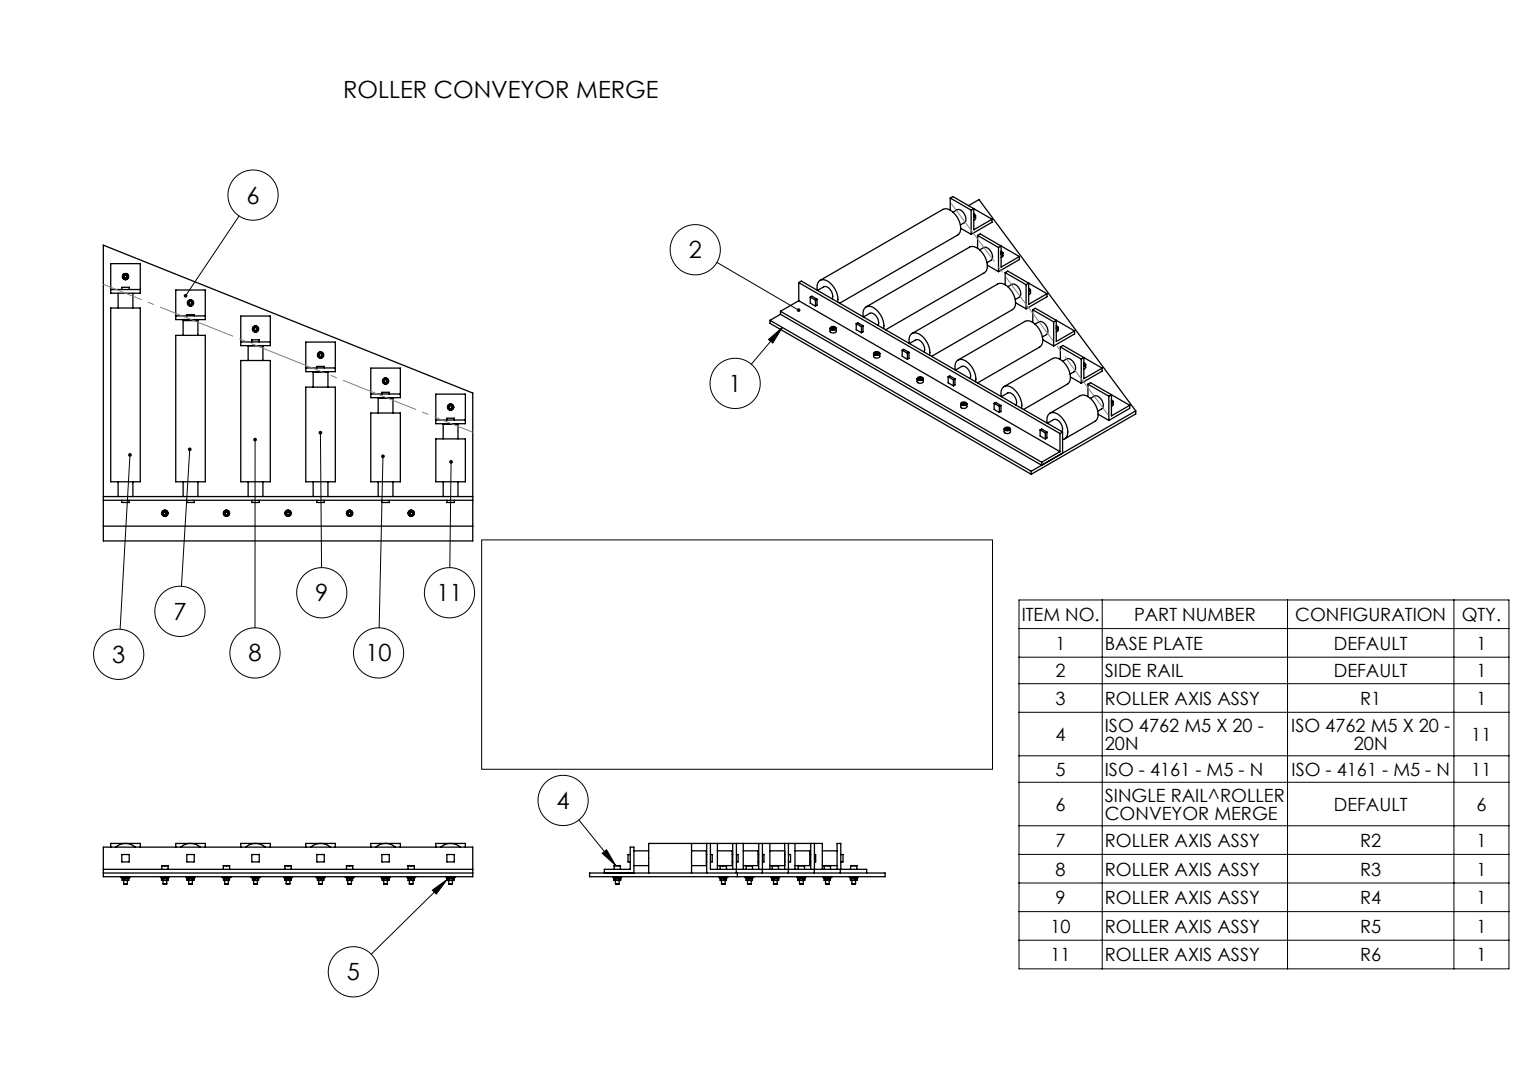
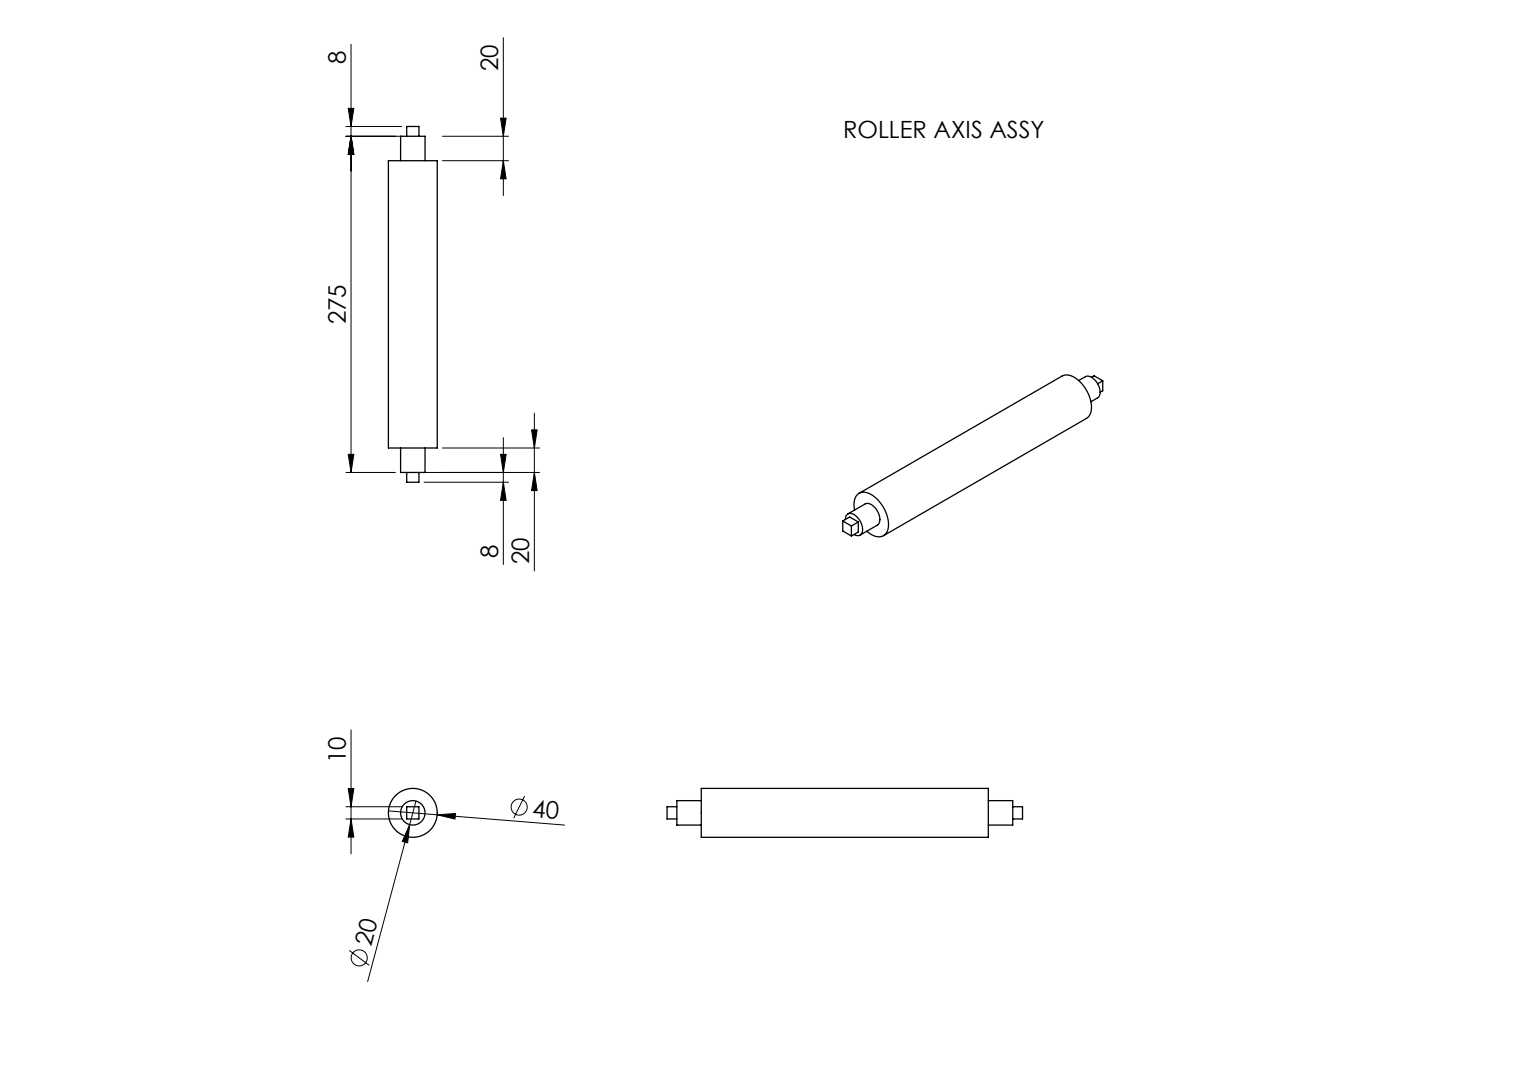
ISO-10303-21;
HEADER;
FILE_DESCRIPTION (('STEP AP214'),
    '1' );
FILE_NAME ('MAS-188',
    '2026-10-24T11:01:53',
    ( '' ),
    ( '' ),
    'SwSTEP 2.0',
    'SolidWorks 2026',
    '' );
FILE_SCHEMA (( 'AUTOMOTIVE_DESIGN' ));
ENDSEC;

DATA;
#1 = FACE_OUTER_BOUND ( 'NONE', #2167, .T. ) ;
#2 = DIRECTION ( 'NONE',  ( 0.000000000000000000, 0.000000000000000000, 1.000000000000000000 ) ) ;
#3 = CARTESIAN_POINT ( 'NONE',  ( 0.000000000000000000, 0.000000000000000000, -4.694516984716113228 ) ) ;
#4 = FILL_AREA_STYLE_COLOUR ( '', #2186 ) ;
#5 = ORIENTED_EDGE ( 'NONE', *, *, #5962, .F. ) ;
#6 = ORIENTED_EDGE ( 'NONE', *, *, #8549, .T. ) ;
#7 = EDGE_CURVE ( 'NONE', #1026, #1114, #8022, .T. ) ;
#8 = ORIENTED_EDGE ( 'NONE', *, *, #6474, .F. ) ;
#9 = APPLICATION_CONTEXT ( 'automotive_design' ) ;
#10 = LINE ( 'NONE', #1868, #5341 ) ;
#11 = EDGE_CURVE ( 'NONE', #6628, #4697, #895, .T. ) ;
#12 = CARTESIAN_POINT ( 'NONE',  ( -5.000000000000000000, -5.000000000000000000, 148.0000000000000284 ) ) ;
#13 = PRODUCT_DEFINITION_FORMATION_WITH_SPECIFIED_SOURCE ( 'ANY', '', #8583, .NOT_KNOWN. ) ;
#14 = EDGE_CURVE ( 'NONE', #3511, #8141, #5542, .T. ) ;
#15 = DIRECTION ( 'NONE',  ( 1.000000000000000000, 0.000000000000000000, 0.000000000000000000 ) ) ;
#16 = ORIENTED_EDGE ( 'NONE', *, *, #5135, .F. ) ;
#17 = LINE ( 'NONE', #599, #1287 ) ;
#18 = CARTESIAN_POINT ( 'NONE',  ( 386.6666666666666288, -15.00000000000000000, 165.1500000000000625 ) ) ;
#19 = FACE_BOUND ( 'NONE', #2899, .T. ) ;
#20 = CARTESIAN_POINT ( 'NONE',  ( 176.0000000000000000, -30.00000000000000355, -86.63142504031549151 ) ) ;
#21 = LINE ( 'NONE', #519, #5740 ) ;
#22 = ORIENTED_EDGE ( 'NONE', *, *, #3719, .T. ) ;
#23 = AXIS2_PLACEMENT_3D ( 'NONE', #2020, #5963, #7409 ) ;
#24 = VERTEX_POINT ( 'NONE', #6412 ) ;
#25 = DIRECTION ( 'NONE',  ( 0.000000000000000000, 0.000000000000000000, 1.000000000000000000 ) ) ;
#26 = CARTESIAN_POINT ( 'NONE',  ( -30.00000000000000000, 15.00000000000000000, 145.0000000000000284 ) ) ;
#27 = AXIS2_PLACEMENT_3D ( 'NONE', #2373, #401, #2287 ) ;
#28 = VECTOR ( 'NONE', #6395, 1000.000000000000000 ) ;
#29 = LINE ( 'NONE', #6648, #3973 ) ;
#30 = EDGE_CURVE ( 'NONE', #66, #5441, #6753, .T. ) ;
#31 = CARTESIAN_POINT ( 'NONE',  ( -4.999999999999998224, -4.999999999999998224, 145.0000000000000284 ) ) ;
#32 = ORIENTED_EDGE ( 'NONE', *, *, #8020, .T. ) ;
#33=STYLED_ITEM('',(#8671),#7573);
#34 = CIRCLE ( 'NONE', #8257, 2.649999999999985700 ) ;
#35 = VERTEX_POINT ( 'NONE', #5063 ) ;
#36 = LINE ( 'NONE', #1308, #2826 ) ;
#37 = AXIS2_PLACEMENT_3D ( 'NONE', #3813, #3117, #8346 ) ;
#38 = MECHANICAL_DESIGN_GEOMETRIC_PRESENTATION_REPRESENTATION (  '', ( #7560 ), #3810 ) ;
#39 = CARTESIAN_POINT ( 'NONE',  ( 264.0000000000000000, -20.00000000000000000, -48.78142504031547588 ) ) ;
#40 = DIRECTION ( 'NONE',  ( 1.000000000000000000, 0.000000000000000000, 0.000000000000000000 ) ) ;
#41 = ORIENTED_EDGE ( 'NONE', *, *, #7818, .F. ) ;
#42 = DIRECTION ( 'NONE',  ( -0.000000000000000000, -0.000000000000000000, 1.000000000000000000 ) ) ;
#43 = VECTOR ( 'NONE', #8305, 1000.000000000000000 ) ;
#44 = DIRECTION ( 'NONE',  ( -1.000000000000000000, 0.000000000000000000, 0.000000000000000000 ) ) ;
#45 = CARTESIAN_POINT ( 'NONE',  ( 352.0000000000000000, -25.00000000000000000, -18.88142504031545243 ) ) ;
#46 = AXIS2_PLACEMENT_3D ( 'NONE', #70, #7390, #6602 ) ;
#47 = CARTESIAN_POINT ( 'NONE',  ( 5.000000000000000000, -5.000000000000000000, 148.0000000000000284 ) ) ;
#48 = VECTOR ( 'NONE', #1988, 1000.000000000000000 ) ;
#49 = CARTESIAN_POINT ( 'NONE',  ( 20.00000000000000000, 0.000000000000000000, 120.0000000000000142 ) ) ;
#50 = DIRECTION ( 'NONE',  ( -0.000000000000000000, 1.000000000000000000, -0.000000000000000000 ) ) ;
#51 = EDGE_LOOP ( 'NONE', ( #1765, #1748 ) ) ;
#52 = EDGE_LOOP ( 'NONE', ( #3037, #7373 ) ) ;
#53 = UNCERTAINTY_MEASURE_WITH_UNIT (LENGTH_MEASURE( 1.000000000000000082E-05 ), #4971, 'distance_accuracy_value', 'NONE');
#54 = VERTEX_POINT ( 'NONE', #1769 ) ;
#55 = DIRECTION ( 'NONE',  ( 1.734723475976806848E-16, -1.000000000000000000, -0.000000000000000000 ) ) ;
#56 = CARTESIAN_POINT ( 'NONE',  ( 10.00000000000000000, 0.000000000000000000, 140.0000000000000000 ) ) ;
#57 = ADVANCED_FACE ( 'NONE', ( #4416 ), #7068, .T. ) ;
#58 = VERTEX_POINT ( 'NONE', #5981 ) ;
#59 = CARTESIAN_POINT ( 'NONE',  ( 5.000000000000000000, -5.000000000000000000, 7.000000000000006217 ) ) ;
#60 = EDGE_CURVE ( 'NONE', #24, #4191, #63, .T. ) ;
#61 = ORIENTED_EDGE ( 'NONE', *, *, #1740, .F. ) ;
#62 = LINE ( 'NONE', #7469, #2279 ) ;
#63 = LINE ( 'NONE', #5464, #2595 ) ;
#64 = CARTESIAN_POINT ( 'NONE',  ( 176.0000000000000000, -10.00000000000000178, -86.63142504031549151 ) ) ;
#65 =( NAMED_UNIT ( * ) PLANE_ANGLE_UNIT ( ) SI_UNIT ( $, .RADIAN. ) );
#66 = VERTEX_POINT ( 'NONE', #8006 ) ;
#67 = EDGE_CURVE ( 'NONE', #3923, #3144, #6728, .T. ) ;
#68 = ORIENTED_EDGE ( 'NONE', *, *, #4489, .T. ) ;
#69 = LINE ( 'NONE', #4867, #7268 ) ;
#70 = CARTESIAN_POINT ( 'NONE',  ( 219.9999999999999716, -14.99999999999999822, 162.5000000000000853 ) ) ;
#71 = CIRCLE ( 'NONE', #3416, 10.00000000000000000 ) ;
#72 = DIRECTION ( 'NONE',  ( 0.000000000000000000, 0.000000000000000000, 1.000000000000000000 ) ) ;
#73 = CARTESIAN_POINT ( 'NONE',  ( 0.000000000000000000, 0.000000000000000000, 140.0000000000000000 ) ) ;
#74 = EDGE_LOOP ( 'NONE', ( #3526, #1411, #5391, #5718 ) ) ;
#75 = CIRCLE ( 'NONE', #7173, 10.00000000000000000 ) ;
#76 = AXIS2_PLACEMENT_3D ( 'NONE', #4160, #6813, #4641 ) ;
#77 = LINE ( 'NONE', #5562, #6140 ) ;
#78 = ORIENTED_EDGE ( 'NONE', *, *, #2299, .F. ) ;
#79 = DIRECTION ( 'NONE',  ( 0.000000000000000000, 0.000000000000000000, 1.000000000000000000 ) ) ;
#80 = CIRCLE ( 'NONE', #1767, 2.649999999999985700 ) ;
#81 = VECTOR ( 'NONE', #7075, 1000.000000000000000 ) ;
#82 = FACE_OUTER_BOUND ( 'NONE', #3870, .T. ) ;
#83 = DIRECTION ( 'NONE',  ( 0.000000000000000000, 1.000000000000000000, -1.224646799147353207E-16 ) ) ;
#84 = ORIENTED_EDGE ( 'NONE', *, *, #5741, .T. ) ;
#85 = DIRECTION ( 'NONE',  ( 0.000000000000000000, 1.000000000000000000, 0.000000000000000000 ) ) ;
#86 = DIRECTION ( 'NONE',  ( -0.000000000000000000, -0.000000000000000000, -1.000000000000000000 ) ) ;
#87 = ADVANCED_FACE ( 'NONE', ( #7344 ), #1423, .F. ) ;
#88 = EDGE_CURVE ( 'NONE', #3290, #1917, #5360, .T. ) ;
#89 = DIRECTION ( 'NONE',  ( -1.000000000000000000, 0.000000000000000000, -0.000000000000000000 ) ) ;
#90 = ADVANCED_FACE ( 'NONE', ( #2733 ), #143, .T. ) ;
#91 = CARTESIAN_POINT ( 'NONE',  ( 0.000000000000000000, 0.000000000000000000, -0.2800830152838844622 ) ) ;
#92 = DIRECTION ( 'NONE',  ( 1.000000000000000000, 0.000000000000000000, 0.000000000000000000 ) ) ;
#93 = FACE_OUTER_BOUND ( 'NONE', #2661, .T. ) ;
#94 = ORIENTED_EDGE ( 'NONE', *, *, #7928, .T. ) ;
#95 = ORIENTED_EDGE ( 'NONE', *, *, #1233, .T. ) ;
#96 = ORIENTED_EDGE ( 'NONE', *, *, #1118, .T. ) ;
#97 = CARTESIAN_POINT ( 'NONE',  ( 10.00000000000000000, 0.000000000000000000, 42.00000000000000711 ) ) ;
#98 = FILL_AREA_STYLE_COLOUR ( '', #4214 ) ;
#99 = EDGE_LOOP ( 'NONE', ( #6356, #2611 ) ) ;
#100 = DIRECTION ( 'NONE',  ( 0.000000000000000000, 0.000000000000000000, -1.000000000000000000 ) ) ;
#101 = VERTEX_POINT ( 'NONE', #4083 ) ;
#102 = CARTESIAN_POINT ( 'NONE',  ( 0.3461262719736147297, -4.658553426539303821, -3.671615880910379381 ) ) ;
#103 = DIRECTION ( 'NONE',  ( 0.000000000000000000, 0.000000000000000000, -1.000000000000000000 ) ) ;
#104 = VERTEX_POINT ( 'NONE', #727 ) ;
#105 = B_SPLINE_CURVE_WITH_KNOTS ( 'NONE', 3,
 ( #4717, #2155, #226, #4890, #3459, #8039 ),
 .UNSPECIFIED., .F., .F.,
 ( 4, 2, 4 ),
 ( 0.003358874760055551890, 0.004541967308452098118, 0.005725059856848645212 ),
 .UNSPECIFIED. ) ;
#106 = ORIENTED_EDGE ( 'NONE', *, *, #3433, .T. ) ;
#107 = CARTESIAN_POINT ( 'NONE',  ( -4.154094228333736538, -2.398367420967545627, -3.721909803043222276 ) ) ;
#108 = CIRCLE ( 'NONE', #2620, 2.649999999999985700 ) ;
#109 = CARTESIAN_POINT ( 'NONE',  ( 2.500000000000000000, -2.357898499370432610, 3.252606517456513302E-15 ) ) ;
#110 = CARTESIAN_POINT ( 'NONE',  ( 0.3208286057739604957, -4.433571671609698228, -0.3503314178412692548 ) ) ;
#111 = AXIS2_PLACEMENT_3D ( 'NONE', #1042, #3694, #1743 ) ;
#112 = CARTESIAN_POINT ( 'NONE',  ( 5.000000000000000000, -5.000000000000000000, -36.00000000000000000 ) ) ;
#113 = ORIENTED_EDGE ( 'NONE', *, *, #5446, .F. ) ;
#114 = CARTESIAN_POINT ( 'NONE',  ( 0.000000000000000000, 0.000000000000000000, 120.0000000000000284 ) ) ;
#115 =( LENGTH_UNIT ( ) NAMED_UNIT ( * ) SI_UNIT ( .MILLI., .METRE. ) );
#116 = LINE ( 'NONE', #6740, #7265 ) ;
#117 = ORIENTED_EDGE ( 'NONE', *, *, #2503, .F. ) ;
#118 = CARTESIAN_POINT ( 'NONE',  ( -2.855764796983342624, 2.970025579236414082, -0.09382832055445475272 ) ) ;
#119 = AXIS2_PLACEMENT_3D ( 'NONE', #4281, #2979, #6929 ) ;
#120 = EDGE_CURVE ( 'NONE', #6932, #5212, #7298, .T. ) ;
#121 = EDGE_CURVE ( 'NONE', #848, #6261, #4955, .T. ) ;
#122 = CARTESIAN_POINT ( 'NONE',  ( 0.000000000000000000, 0.000000000000000000, -4.974599999999998801 ) ) ;
#123 = DIRECTION ( 'NONE',  ( 0.000000000000000000, -0.000000000000000000, 1.000000000000000000 ) ) ;
#124 = ORIENTED_EDGE ( 'NONE', *, *, #3492, .T. ) ;
#125 = LINE ( 'NONE', #5958, #4603 ) ;
#126 = AXIS2_PLACEMENT_3D ( 'NONE', #2068, #2105, #1941 ) ;
#127 = DIRECTION ( 'NONE',  ( 0.000000000000000000, 0.000000000000000000, 1.000000000000000000 ) ) ;
#128 = CARTESIAN_POINT ( 'NONE',  ( 5.000000000000000000, -5.000000000000000000, 34.00000000000000711 ) ) ;
#129 = FACE_OUTER_BOUND ( 'NONE', #369, .T. ) ;
#130 = LINE ( 'NONE', #5451, #8061 ) ;
#131 = DIRECTION ( 'NONE',  ( 0.5000000000000013323, -0.8660254037844379305, 0.000000000000000000 ) ) ;
#132 = ADVANCED_FACE ( 'NONE', ( #686, #1511 ), #6069, .T. ) ;
#133 = VERTEX_POINT ( 'NONE', #5381 ) ;
#134 = ORIENTED_EDGE ( 'NONE', *, *, #577, .F. ) ;
#135 = EDGE_LOOP ( 'NONE', ( #1108, #6424, #4835, #16 ) ) ;
#136 = CARTESIAN_POINT ( 'NONE',  ( 5.200000000000002842, 0.000000000000000000, 0.000000000000000000 ) ) ;
#137 =( NAMED_UNIT ( * ) PLANE_ANGLE_UNIT ( ) SI_UNIT ( $, .RADIAN. ) );
#138 = AXIS2_PLACEMENT_3D ( 'NONE', #293, #6173, #2138 ) ;
#139 = ORIENTED_EDGE ( 'NONE', *, *, #5913, .F. ) ;
#140 = LINE ( 'NONE', #6246, #2728 ) ;
#141 = ORIENTED_EDGE ( 'NONE', *, *, #4885, .F. ) ;
#142 = CARTESIAN_POINT ( 'NONE',  ( 0.000000000000000000, 157.5000000000000284, 0.000000000000000000 ) ) ;
#143 = CYLINDRICAL_SURFACE ( 'NONE', #76, 20.00000000000000000 ) ;
#144 = CONTEXT_DEPENDENT_SHAPE_REPRESENTATION ( #1867, #2670 ) ;
#145 =( NAMED_UNIT ( * ) SI_UNIT ( $, .STERADIAN. ) SOLID_ANGLE_UNIT ( ) );
#146 = ORIENTED_EDGE ( 'NONE', *, *, #2955, .F. ) ;
#147 = VERTEX_POINT ( 'NONE', #2776 ) ;
#148 = AXIS2_PLACEMENT_3D ( 'NONE', #7664, #476, #5775 ) ;
#149 = CARTESIAN_POINT ( 'NONE',  ( -30.00000000000002842, -15.00000000000000000, 180.0000000000000284 ) ) ;
#150 = AXIS2_PLACEMENT_3D ( 'NONE', #5383, #907, #6207 ) ;
#151 = CARTESIAN_POINT ( 'NONE',  ( 264.0000000000000000, -20.00000000000000000, -51.43142504031546025 ) ) ;
#152 = CARTESIAN_POINT ( 'NONE',  ( 0.000000000000000000, -20.00000000000000000, -154.8500000000000512 ) ) ;
#153 = PRODUCT_DEFINITION_SHAPE ( 'NONE', 'NONE',  #1825 ) ;
#154 = CARTESIAN_POINT ( 'NONE',  ( 0.5469614295415388128, -4.303013824935362663, -3.535263753543555598 ) ) ;
#155 = ORIENTED_EDGE ( 'NONE', *, *, #8498, .T. ) ;
#156 = VECTOR ( 'NONE', #5813, 1000.000000000000000 ) ;
#157 = CARTESIAN_POINT ( 'NONE',  ( -5.000000000000001776, 5.000000000000001776, -36.00000000000000000 ) ) ;
#158 = CARTESIAN_POINT ( 'NONE',  ( -5.000000000000001776, 5.000000000000001776, 34.00000000000000711 ) ) ;
#159 = EDGE_LOOP ( 'NONE', ( #3695, #3628, #3551, #216 ) ) ;
#160 = CIRCLE ( 'NONE', #1848, 10.00000000000000000 ) ;
#161 = DIRECTION ( 'NONE',  ( -1.000000000000000000, 0.000000000000000000, 0.000000000000000000 ) ) ;
#162 = DIRECTION ( 'NONE',  ( -0.000000000000000000, -0.000000000000000000, 1.000000000000000000 ) ) ;
#163 = AXIS2_PLACEMENT_3D ( 'NONE', #2738, #6866, #8185 ) ;
#164 = CIRCLE ( 'NONE', #2122, 10.00000000000000000 ) ;
#165 = AXIS2_PLACEMENT_3D ( 'NONE', #4222, #789, #916 ) ;
#166 = CARTESIAN_POINT ( 'NONE',  ( 20.00000000000000000, 0.000000000000000000, -7.999999999999992895 ) ) ;
#167 = ADVANCED_FACE ( 'NONE', ( #3513 ), #4000, .F. ) ;
#168 = LINE ( 'NONE', #4141, #8472 ) ;
#169 = EDGE_LOOP ( 'NONE', ( #5952, #1913, #7757, #4086 ) ) ;
#170 = DIRECTION ( 'NONE',  ( -1.000000000000000000, 0.000000000000000000, -0.000000000000000000 ) ) ;
#171 = VECTOR ( 'NONE', #2949, 1000.000000000000000 ) ;
#172 = EDGE_CURVE ( 'NONE', #3127, #1490, #6613, .T. ) ;
#173 = VECTOR ( 'NONE', #7716, 1000.000000000000000 ) ;
#174 = DIRECTION ( 'NONE',  ( 0.000000000000000000, -1.000000000000000000, 0.000000000000000000 ) ) ;
#175 = EDGE_CURVE ( 'NONE', #7885, #4775, #2327, .T. ) ;
#176 = VECTOR ( 'NONE', #5079, 1000.000000000000000 ) ;
#177 =( GEOMETRIC_REPRESENTATION_CONTEXT ( 3 ) GLOBAL_UNCERTAINTY_ASSIGNED_CONTEXT ( ( #6671 ) ) GLOBAL_UNIT_ASSIGNED_CONTEXT ( ( #6629, #7289, #586 ) ) REPRESENTATION_CONTEXT ( 'NONE', 'WORKASPACE' ) );
#178 = DIRECTION ( 'NONE',  ( -0.000000000000000000, -0.000000000000000000, 1.000000000000000000 ) ) ;
#179 = APPLICATION_CONTEXT ( 'automotive_design' ) ;
#180 = FACE_OUTER_BOUND ( 'NONE', #6238, .T. ) ;
#181 = CARTESIAN_POINT ( 'NONE',  ( -0.5449313310646672903, -4.304185902836978883, -3.316620875263469159 ) ) ;
#182 = CARTESIAN_POINT ( 'NONE',  ( 269.0000000000000000, -4.999999999999998224, 145.0000000000000284 ) ) ;
#183 = AXIS2_PLACEMENT_3D ( 'NONE', #2227, #4879, #1572 ) ;
#184 = ORIENTED_EDGE ( 'NONE', *, *, #1602, .F. ) ;
#185 = ORIENTED_EDGE ( 'NONE', *, *, #253, .T. ) ;
#186 = VERTEX_POINT ( 'NONE', #5337 ) ;
#187 = CARTESIAN_POINT ( 'NONE',  ( -10.00000000000000000, 1.224646799147353256E-15, 42.00000000000000711 ) ) ;
#188 = AXIS2_PLACEMENT_3D ( 'NONE', #1470, #2312, #5600 ) ;
#189 = EDGE_CURVE ( 'NONE', #7561, #1754, #4818, .T. ) ;
#190 = ORIENTED_EDGE ( 'NONE', *, *, #4626, .T. ) ;
#191 = FACE_OUTER_BOUND ( 'NONE', #6163, .T. ) ;
#192 = EDGE_LOOP ( 'NONE', ( #1418, #8130, #7597, #2442 ) ) ;
#193 = CARTESIAN_POINT ( 'NONE',  ( -4.999999999999998224, 135.0000000000000000, 25.00000000000000000 ) ) ;
#194 = DIRECTION ( 'NONE',  ( -1.000000000000000000, 0.000000000000000000, 0.000000000000000000 ) ) ;
#195 = ORIENTED_EDGE ( 'NONE', *, *, #2103, .T. ) ;
#196 = AXIS2_PLACEMENT_3D ( 'NONE', #7241, #2034, #5327 ) ;
#197 = ORIENTED_EDGE ( 'NONE', *, *, #8549, .F. ) ;
#198 = CARTESIAN_POINT ( 'NONE',  ( -10.00000000000000000, 1.224646799147353256E-15, 120.0000000000000142 ) ) ;
#199 = LINE ( 'NONE', #109, #2686 ) ;
#200 = EDGE_CURVE ( 'NONE', #6574, #3690, #7176, .T. ) ;
#201 = EDGE_CURVE ( 'NONE', #7722, #4892, #6771, .T. ) ;
#202 = EDGE_CURVE ( 'NONE', #3923, #6024, #3423, .T. ) ;
#203 = LINE ( 'NONE', #2266, #5375 ) ;
#204 = DIRECTION ( 'NONE',  ( 0.000000000000000000, -0.000000000000000000, 1.000000000000000000 ) ) ;
#205 = EDGE_LOOP ( 'NONE', ( #3377, #2708, #3333, #2786 ) ) ;
#206 = SURFACE_SIDE_STYLE ('',( #4174 ) ) ;
#207 = CARTESIAN_POINT ( 'NONE',  ( 10.00000000000000000, 0.000000000000000000, 140.0000000000000000 ) ) ;
#208 = ORIENTED_EDGE ( 'NONE', *, *, #6764, .T. ) ;
#209 = AXIS2_PLACEMENT_3D ( 'NONE', #6688, #3397, #6036 ) ;
#210 = DIRECTION ( 'NONE',  ( 0.5000000000000022204, 0.8660254037844374864, -0.000000000000000000 ) ) ;
#211 = AXIS2_PLACEMENT_3D ( 'NONE', #7037, #7745, #1783 ) ;
#212 = DIRECTION ( 'NONE',  ( 0.000000000000000000, 1.000000000000000000, -1.471414886128461471E-15 ) ) ;
#213 = AXIS2_PLACEMENT_3D ( 'NONE', #3905, #5378, #2079 ) ;
#214 = CARTESIAN_POINT ( 'NONE',  ( 24.55500000000002103, 3.061616997868384620E-16, -2.500000000000001332 ) ) ;
#215 = FACE_OUTER_BOUND ( 'NONE', #5011, .T. ) ;
#216 = ORIENTED_EDGE ( 'NONE', *, *, #6684, .T. ) ;
#217 = CARTESIAN_POINT ( 'NONE',  ( -1.393927851585477606, 4.043713361053528743, -3.526374918436835149 ) ) ;
#218 = PRESENTATION_STYLE_ASSIGNMENT (( #6840 ) ) ;
#219 = CARTESIAN_POINT ( 'NONE',  ( 386.6666666666666288, -20.00000000000000000, 162.5000000000000853 ) ) ;
#220 = AXIS2_PLACEMENT_3D ( 'NONE', #6944, #7654, #6292 ) ;
#221 = CARTESIAN_POINT ( 'NONE',  ( 5.000000000000000000, 5.000000000000000000, 140.0000000000000000 ) ) ;
#222 = DIRECTION ( 'NONE',  ( -0.000000000000000000, -0.000000000000000000, -1.000000000000000000 ) ) ;
#223 = ADVANCED_FACE ( 'NONE', ( #1998, #2816 ), #373, .T. ) ;
#224 = PRESENTATION_LAYER_ASSIGNMENT (  '', '', ( #651 ) ) ;
#225 = CARTESIAN_POINT ( 'NONE',  ( -4.175002511812151873, -2.208363329454905877, -3.469254087858246738 ) ) ;
#226 = CARTESIAN_POINT ( 'NONE',  ( 4.000000000000000000, -1.560351142792952617, -0.2242961665059816367 ) ) ;
#227 = AXIS2_PLACEMENT_3D ( 'NONE', #2062, #2145, #1353 ) ;
#228 = ORIENTED_EDGE ( 'NONE', *, *, #2374, .T. ) ;
#229 = ORIENTED_EDGE ( 'NONE', *, *, #1735, .F. ) ;
#230 = DIRECTION ( 'NONE',  ( -0.000000000000000000, -0.000000000000000000, 1.000000000000000000 ) ) ;
#231 = CARTESIAN_POINT ( 'NONE',  ( -5.000000000000000000, -5.000000000000000000, -0.9999999999999940048 ) ) ;
#232 = DIRECTION ( 'NONE',  ( 0.000000000000000000, -0.000000000000000000, 1.000000000000000000 ) ) ;
#233 = PRODUCT_DEFINITION_SHAPE ( 'NONE', 'NONE',  #8625 ) ;
#234 = EDGE_CURVE ( 'NONE', #3505, #4164, #2178, .T. ) ;
#235 = EDGE_CURVE ( 'NONE', #6809, #4852, #8223, .T. ) ;
#236 = ORIENTED_EDGE ( 'NONE', *, *, #2533, .T. ) ;
#237 = DIRECTION ( 'NONE',  ( 0.000000000000000000, -0.4999999999999993894, 0.8660254037844389297 ) ) ;
#238 = VERTEX_POINT ( 'NONE', #4948 ) ;
#239 = DIRECTION ( 'NONE',  ( -0.000000000000000000, -0.000000000000000000, -1.000000000000000000 ) ) ;
#240 = DIRECTION ( 'NONE',  ( -0.000000000000000000, -0.000000000000000000, 1.000000000000000000 ) ) ;
#241 = DIRECTION ( 'NONE',  ( 0.000000000000000000, 0.000000000000000000, 1.000000000000000000 ) ) ;
#242 = VERTEX_POINT ( 'NONE', #1553 ) ;
#243 = VERTEX_POINT ( 'NONE', #1034 ) ;
#244 = FACE_OUTER_BOUND ( 'NONE', #4831, .T. ) ;
#245 = LINE ( 'NONE', #4910, #2842 ) ;
#246 = DIRECTION ( 'NONE',  ( 0.000000000000000000, 1.000000000000000000, 0.000000000000000000 ) ) ;
#247 = PLANE ( 'NONE',  #2215 ) ;
#248 = ORIENTED_EDGE ( 'NONE', *, *, #3329, .F. ) ;
#249 = EDGE_CURVE ( 'NONE', #7704, #6568, #408, .T. ) ;
#250 = AXIS2_PLACEMENT_3D ( 'NONE', #5052, #3664, #1753 ) ;
#251 = DIRECTION ( 'NONE',  ( -0.000000000000000000, -0.000000000000000000, 1.000000000000000000 ) ) ;
#252 = ORIENTED_EDGE ( 'NONE', *, *, #8466, .T. ) ;
#253 = EDGE_CURVE ( 'NONE', #1917, #3290, #7040, .T. ) ;
#254 = ORIENTED_EDGE ( 'NONE', *, *, #6075, .T. ) ;
#255 = DIRECTION ( 'NONE',  ( 0.000000000000000000, -1.000000000000000000, 0.000000000000000000 ) ) ;
#256 = CARTESIAN_POINT ( 'NONE',  ( 0.000000000000000000, -1.178949249685213863, 2.042000000000002924 ) ) ;
#257 = AXIS2_PLACEMENT_3D ( 'NONE', #4957, #2556, #3896 ) ;
#258 = DIRECTION ( 'NONE',  ( -0.000000000000000000, 0.000000000000000000, 1.000000000000000000 ) ) ;
#259 = DIRECTION ( 'NONE',  ( 0.000000000000000000, 0.000000000000000000, 1.000000000000000000 ) ) ;
#260 = ORIENTED_EDGE ( 'NONE', *, *, #2345, .F. ) ;
#261 = FACE_OUTER_BOUND ( 'NONE', #2202, .T. ) ;
#262 = FILL_AREA_STYLE_COLOUR ( '', #7978 ) ;
#263 = VECTOR ( 'NONE', #6923, 1000.000000000000000 ) ;
#264 = CARTESIAN_POINT ( 'NONE',  ( -6.259644161404860030E-16, -4.618802153517027165, -5.000000000000000000 ) ) ;
#265 = PRODUCT_RELATED_PRODUCT_CATEGORY ( 'part', '', ( #1494 ) ) ;
#266 = CARTESIAN_POINT ( 'NONE',  ( -20.00000000000000000, 135.0000000000000000, 40.00000000000000000 ) ) ;
#267 = DIRECTION ( 'NONE',  ( 0.000000000000000000, 0.000000000000000000, 1.000000000000000000 ) ) ;
#268 = CARTESIAN_POINT ( 'NONE',  ( 0.000000000000000000, -2.357898499370432610, 3.252606517456513302E-15 ) ) ;
#269 = DIRECTION ( 'NONE',  ( -1.000000000000000000, 0.000000000000000000, 0.000000000000000000 ) ) ;
#270 = ORIENTED_EDGE ( 'NONE', *, *, #6348, .F. ) ;
#271 = ORIENTED_EDGE ( 'NONE', *, *, #4539, .T. ) ;
#272 = ORIENTED_EDGE ( 'NONE', *, *, #334, .T. ) ;
#273 = LINE ( 'NONE', #2937, #2703 ) ;
#274 = AXIS2_PLACEMENT_3D ( 'NONE', #7086, #7713, #1130 ) ;
#275 = AXIS2_PLACEMENT_3D ( 'NONE', #2564, #1326, #1164 ) ;
#276 = LINE ( 'NONE', #6936, #1165 ) ;
#277 = ORIENTED_EDGE ( 'NONE', *, *, #6684, .F. ) ;
#278 = DIRECTION ( 'NONE',  ( 0.000000000000000000, 0.000000000000000000, -1.000000000000000000 ) ) ;
#279 = EDGE_CURVE ( 'NONE', #5674, #3807, #5550, .T. ) ;
#280 = EDGE_LOOP ( 'NONE', ( #1138, #316, #2891, #6208 ) ) ;
#281 = DIRECTION ( 'NONE',  ( 0.000000000000000000, 0.000000000000000000, 1.000000000000000000 ) ) ;
#282 = EDGE_CURVE ( 'NONE', #4949, #5455, #6249, .T. ) ;
#283 = APPLICATION_PROTOCOL_DEFINITION ( 'draft international standard', 'automotive_design', 1998, #4186 ) ;
#284 = ORIENTED_EDGE ( 'NONE', *, *, #8567, .F. ) ;
#285 = B_SPLINE_CURVE_WITH_KNOTS ( 'NONE', 3,
 ( #8294, #4931, #1495, #2332, #6091, #6272 ),
 .UNSPECIFIED., .F., .F.,
 ( 4, 2, 4 ),
 ( 0.002365888236228001588, 0.003551327329835089319, 0.004736766423442177049 ),
 .UNSPECIFIED. ) ;
#286 = EDGE_LOOP ( 'NONE', ( #7427, #1240, #4470, #6347 ) ) ;
#287 = PLANE ( 'NONE',  #7700 ) ;
#288 = EDGE_CURVE ( 'NONE', #3976, #6369, #1904, .T. ) ;
#289 = CARTESIAN_POINT ( 'NONE',  ( 219.9999999999999716, -20.00000000000000000, 165.1500000000000625 ) ) ;
#290 = FACE_OUTER_BOUND ( 'NONE', #6194, .T. ) ;
#291 = CARTESIAN_POINT ( 'NONE',  ( 4.211140560182196957, 2.431303136016536470, -3.745885042887433514 ) ) ;
#292 = ORIENTED_EDGE ( 'NONE', *, *, #6462, .T. ) ;
#293 = CARTESIAN_POINT ( 'NONE',  ( 0.000000000000000000, 0.000000000000000000, 0.000000000000000000 ) ) ;
#294 = DIRECTION ( 'NONE',  ( 1.000000000000000000, 1.734723475976806848E-16, 0.000000000000000000 ) ) ;
#295 = EDGE_LOOP ( 'NONE', ( #7507, #2657, #3424, #1885 ) ) ;
#296 = EDGE_LOOP ( 'NONE', ( #5180, #2362, #7003, #1502 ) ) ;
#297 = DIRECTION ( 'NONE',  ( 0.000000000000000000, 0.000000000000000000, -1.000000000000000000 ) ) ;
#298 = DIRECTION ( 'NONE',  ( 0.000000000000000000, 0.000000000000000000, 1.000000000000000000 ) ) ;
#299 = EDGE_CURVE ( 'NONE', #6060, #4780, #4987, .T. ) ;
#300 = PRODUCT_DEFINITION_FORMATION_WITH_SPECIFIED_SOURCE ( 'ANY', '', #7393, .NOT_KNOWN. ) ;
#301 = AXIS2_PLACEMENT_3D ( 'NONE', #6411, #4498, #8473 ) ;
#302 = B_SPLINE_CURVE_WITH_KNOTS ( 'NONE', 3,
 ( #1517, #107, #2781, #5426, #8101, #4823 ),
 .UNSPECIFIED., .F., .F.,
 ( 4, 2, 4 ),
 ( -3.640115492409406142E-06, 0.0002066546034006526487, 0.0004169493222937146744 ),
 .UNSPECIFIED. ) ;
#303 = FACE_BOUND ( 'NONE', #4384, .T. ) ;
#304 = CARTESIAN_POINT ( 'NONE',  ( 0.000000000000000000, 0.000000000000000000, 7.000000000000006217 ) ) ;
#305 = ORIENTED_EDGE ( 'NONE', *, *, #3009, .T. ) ;
#306 = EDGE_CURVE ( 'NONE', #5455, #35, #2943, .T. ) ;
#307 = DIRECTION ( 'NONE',  ( -1.000000000000000000, 0.000000000000000000, 0.000000000000000000 ) ) ;
#308 = AXIS2_PLACEMENT_3D ( 'NONE', #6873, #251, #6040 ) ;
#309 = DIRECTION ( 'NONE',  ( 0.000000000000000000, 0.000000000000000000, 1.000000000000000000 ) ) ;
#310 = AXIS2_PLACEMENT_3D ( 'NONE', #6705, #757, #2626 ) ;
#311 = DIRECTION ( 'NONE',  ( 1.000000000000000000, 0.000000000000000000, 0.000000000000000000 ) ) ;
#312 = AXIS2_PLACEMENT_3D ( 'NONE', #2273, #7297, #3257 ) ;
#313 = CARTESIAN_POINT ( 'NONE',  ( 2.500000000000000000, 0.000000000000000000, 0.000000000000000000 ) ) ;
#314 = VECTOR ( 'NONE', #3349, 999.9999999999998863 ) ;
#315 = CARTESIAN_POINT ( 'NONE',  ( 0.02511973781850649831, -4.877415612947427981, -3.751298745799844792 ) ) ;
#316 = ORIENTED_EDGE ( 'NONE', *, *, #4226, .F. ) ;
#317 = CIRCLE ( 'NONE', #5184, 20.00000000000000000 ) ;
#318 = ORIENTED_EDGE ( 'NONE', *, *, #3170, .T. ) ;
#319 = ORIENTED_EDGE ( 'NONE', *, *, #4563, .T. ) ;
#320 = FACE_OUTER_BOUND ( 'NONE', #6882, .T. ) ;
#321 = LINE ( 'NONE', #6328, #6444 ) ;
#322 = VECTOR ( 'NONE', #5585, 1000.000000000000000 ) ;
#323 = ORIENTED_EDGE ( 'NONE', *, *, #2666, .F. ) ;
#324 = DIRECTION ( 'NONE',  ( -0.000000000000000000, -0.000000000000000000, -1.000000000000000000 ) ) ;
#325 = EDGE_LOOP ( 'NONE', ( #5530, #4700, #8320, #94 ) ) ;
#326 = CARTESIAN_POINT ( 'NONE',  ( 5.000000000000000000, -5.000000000000000000, -143.0000000000000284 ) ) ;
#327 = ITEM_DEFINED_TRANSFORMATION ( 'NONE', 'NONE', #2258,  #594 ) ;
#328 = ORIENTED_EDGE ( 'NONE', *, *, #4280, .F. ) ;
#329 = ADVANCED_FACE ( 'NONE', ( #2350 ), #2992, .T. ) ;
#330 = ORIENTED_EDGE ( 'NONE', *, *, #5204, .F. ) ;
#331 = AXIS2_PLACEMENT_3D ( 'NONE', #650, #3395, #2654 ) ;
#332 = FACE_BOUND ( 'NONE', #3831, .T. ) ;
#333 = CARTESIAN_POINT ( 'NONE',  ( 170.9999999999999716, 5.000000000000001776, 140.0000000000000000 ) ) ;
#334 = EDGE_CURVE ( 'NONE', #2939, #4339, #7033, .T. ) ;
#335 = CARTESIAN_POINT ( 'NONE',  ( 5.000000000000000000, -5.000000000000000000, 140.0000000000000000 ) ) ;
#336 = DIRECTION ( 'NONE',  ( 1.000000000000000000, 0.000000000000000000, 0.000000000000000000 ) ) ;
#337 = VERTEX_POINT ( 'NONE', #8267 ) ;
#338 = EDGE_CURVE ( 'NONE', #2469, #1525, #4337, .T. ) ;
#339 = CARTESIAN_POINT ( 'NONE',  ( 264.0000000000000000, -20.00000000000000000, 106.0685749596845682 ) ) ;
#340 = PLANE ( 'NONE',  #5145 ) ;
#341 = ORIENTED_EDGE ( 'NONE', *, *, #4565, .T. ) ;
#342 = VERTEX_POINT ( 'NONE', #5637 ) ;
#343 = DIRECTION ( 'NONE',  ( -0.000000000000000000, -0.000000000000000000, 1.000000000000000000 ) ) ;
#344 = CARTESIAN_POINT ( 'NONE',  ( 20.00000000000000000, 0.000000000000000000, 120.0000000000000142 ) ) ;
#345 = DIRECTION ( 'NONE',  ( 0.000000000000000000, 1.000000000000000000, 0.000000000000000000 ) ) ;
#346 = CARTESIAN_POINT ( 'NONE',  ( 5.000000000000000000, 5.000000000000000000, 140.0000000000000000 ) ) ;
#347 = ORIENTED_EDGE ( 'NONE', *, *, #4193, .T. ) ;
#348 = PLANE ( 'NONE',  #2219 ) ;
#349 =( LENGTH_UNIT ( ) NAMED_UNIT ( * ) SI_UNIT ( .MILLI., .METRE. ) );
#350 = ORIENTED_EDGE ( 'NONE', *, *, #4139, .T. ) ;
#351 = APPLICATION_CONTEXT ( 'automotive_design' ) ;
#352 = CARTESIAN_POINT ( 'NONE',  ( -5.000000000000001776, 5.000000000000001776, -135.0000000000000000 ) ) ;
#353 = FACE_OUTER_BOUND ( 'NONE', #1557, .T. ) ;
#354 = CIRCLE ( 'NONE', #2031, 2.649999999999993694 ) ;
#355 = DIRECTION ( 'NONE',  ( 1.000000000000000000, 0.000000000000000000, 0.000000000000000000 ) ) ;
#356 = CARTESIAN_POINT ( 'NONE',  ( 5.000000000000000000, -5.000000000000000000, -97.99999999999997158 ) ) ;
#357 = DIRECTION ( 'NONE',  ( 1.734723475976806848E-16, -1.000000000000000000, -0.000000000000000000 ) ) ;
#358 = ORIENTED_EDGE ( 'NONE', *, *, #189, .F. ) ;
#359 = CIRCLE ( 'NONE', #3284, 2.649999999999985700 ) ;
#360 = ORIENTED_EDGE ( 'NONE', *, *, #4499, .F. ) ;
#361 = ADVANCED_FACE ( 'NONE', ( #4903 ), #2861, .F. ) ;
#362 = VECTOR ( 'NONE', #6205, 1000.000000000000000 ) ;
#363 = EDGE_CURVE ( 'NONE', #6062, #5755, #7748, .T. ) ;
#364 = CARTESIAN_POINT ( 'NONE',  ( 2.000000000000005329, -3.464101615137751722, 0.000000000000000000 ) ) ;
#365 = DIRECTION ( 'NONE',  ( -1.000000000000000000, 0.000000000000000000, 0.000000000000000000 ) ) ;
#366 = CARTESIAN_POINT ( 'NONE',  ( 5.000000000000000000, -5.000000000000000000, 42.00000000000000711 ) ) ;
#367 = AXIS2_PLACEMENT_3D ( 'NONE', #5408, #1407, #4068 ) ;
#368 = CONICAL_SURFACE ( 'NONE', #4533, 2.500000000000000888, 0.9599310885968785900 ) ;
#369 = EDGE_LOOP ( 'NONE', ( #8179, #7657, #2904, #5025 ) ) ;
#370 = SURFACE_STYLE_FILL_AREA ( #2990 ) ;
#371 = ORIENTED_EDGE ( 'NONE', *, *, #7980, .T. ) ;
#372 = SURFACE_STYLE_USAGE ( .BOTH. , #1644 ) ;
#373 = PLANE ( 'NONE',  #8303 ) ;
#374 = CONTEXT_DEPENDENT_SHAPE_REPRESENTATION ( #3631, #4419 ) ;
#375 = ORIENTED_EDGE ( 'NONE', *, *, #4660, .F. ) ;
#376 = ORIENTED_EDGE ( 'NONE', *, *, #8589, .T. ) ;
#377 = DIRECTION ( 'NONE',  ( -1.000000000000000000, -0.000000000000000000, -0.000000000000000000 ) ) ;
#378 = EDGE_CURVE ( 'NONE', #2201, #8486, #3600, .T. ) ;
#379 = DIRECTION ( 'NONE',  ( -0.000000000000000000, -0.000000000000000000, 1.000000000000000000 ) ) ;
#380 = CARTESIAN_POINT ( 'NONE',  ( 0.000000000000000000, 0.000000000000000000, -7.999999999999996447 ) ) ;
#381 = DIRECTION ( 'NONE',  ( 1.734723475976806848E-16, -1.000000000000000000, -0.000000000000000000 ) ) ;
#382 = EDGE_LOOP ( 'NONE', ( #940, #229 ) ) ;
#383 = DIRECTION ( 'NONE',  ( 6.123233995736766036E-17, -1.000000000000000000, 0.000000000000000000 ) ) ;
#384 = DIRECTION ( 'NONE',  ( 0.000000000000000000, 0.000000000000000000, -1.000000000000000000 ) ) ;
#385 = ORIENTED_EDGE ( 'NONE', *, *, #7155, .F. ) ;
#386 = ORIENTED_EDGE ( 'NONE', *, *, #234, .T. ) ;
#387 = LINE ( 'NONE', #1178, #6990 ) ;
#388 = LINE ( 'NONE', #2410, #2981 ) ;
#389 = CARTESIAN_POINT ( 'NONE',  ( 2.500000000000000000, 1.178949249685213863, -2.042000000000001148 ) ) ;
#390 = AXIS2_PLACEMENT_3D ( 'NONE', #5308, #6267, #5487 ) ;
#391 = DIRECTION ( 'NONE',  ( 1.000000000000000000, 0.000000000000000000, 0.000000000000000000 ) ) ;
#392 = VERTEX_POINT ( 'NONE', #5029 ) ;
#393 = ADVANCED_FACE ( 'NONE', ( #1075, #7701 ), #3728, .F. ) ;
#394 = PRESENTATION_STYLE_ASSIGNMENT (( #714 ) ) ;
#395 = ORIENTED_EDGE ( 'NONE', *, *, #4970, .F. ) ;
#396 = CARTESIAN_POINT ( 'NONE',  ( -0.02511973781850462134, 4.877415612947412882, -3.751298745799839462 ) ) ;
#397 = ADVANCED_FACE ( 'NONE', ( #5238 ), #7161, .F. ) ;
#398 = B_SPLINE_CURVE_WITH_KNOTS ( 'NONE', 3,
 ( #1284, #3902, #6544, #5158, #1908 ),
 .UNSPECIFIED., .F., .F.,
 ( 4, 1, 4 ),
 ( 0.000000000000000000, 0.002309401076758505356, 0.004618802153517010713 ),
 .UNSPECIFIED. ) ;
#399 = AXIS2_PLACEMENT_3D ( 'NONE', #8232, #5559, #1521 ) ;
#400 = EDGE_CURVE ( 'NONE', #4773, #8282, #7861, .T. ) ;
#401 = DIRECTION ( 'NONE',  ( -0.000000000000000000, 0.8660254037844390407, 0.4999999999999993339 ) ) ;
#402 = PLANE ( 'NONE',  #6759 ) ;
#403 = LINE ( 'NONE', #6405, #2228 ) ;
#404 = FACE_OUTER_BOUND ( 'NONE', #903, .T. ) ;
#405 =( LENGTH_UNIT ( ) NAMED_UNIT ( * ) SI_UNIT ( .MILLI., .METRE. ) );
#406 = AXIS2_PLACEMENT_3D ( 'NONE', #5690, #1942, #2315 ) ;
#407 = ORIENTED_EDGE ( 'NONE', *, *, #3455, .T. ) ;
#408 = LINE ( 'NONE', #3556, #5504 ) ;
#409 = CARTESIAN_POINT ( 'NONE',  ( -3.264650091097280831E-13, -4.796980096169642493, -3.721999068284424617 ) ) ;
#410 = CARTESIAN_POINT ( 'NONE',  ( 10.00000000000000000, 0.000000000000000000, 42.00000000000000711 ) ) ;
#411 = AXIS2_PLACEMENT_3D ( 'NONE', #7547, #5624, #7640 ) ;
#412 = ADVANCED_FACE ( 'NONE', ( #1906, #505 ), #7904, .T. ) ;
#413 = ORIENTED_EDGE ( 'NONE', *, *, #6908, .F. ) ;
#414 = DIRECTION ( 'NONE',  ( -0.000000000000000000, 1.000000000000000000, -0.000000000000000000 ) ) ;
#415 = ORIENTED_EDGE ( 'NONE', *, *, #2060, .F. ) ;
#416 = SURFACE_STYLE_FILL_AREA ( #6943 ) ;
#417 = CARTESIAN_POINT ( 'NONE',  ( 0.000000000000000000, -20.00000000000000000, -157.5000000000000284 ) ) ;
#418 = ITEM_DEFINED_TRANSFORMATION ( 'NONE', 'NONE', #6416,  #594 ) ;
#419 = EDGE_LOOP ( 'NONE', ( #6359, #5460, #4136, #4345 ) ) ;
#420 = ORIENTED_EDGE ( 'NONE', *, *, #3116, .F. ) ;
#421 = FACE_BOUND ( 'NONE', #6148, .T. ) ;
#422 = CARTESIAN_POINT ( 'NONE',  ( -5.000000000000000000, -5.000000000000000000, -71.99999999999998579 ) ) ;
#423 = CARTESIAN_POINT ( 'NONE',  ( 4.207491450040567571, -2.029819825146485179, -3.671670828759567407 ) ) ;
#424 = PRODUCT_DEFINITION ( 'UNKNOWN', '', #7110, #637 ) ;
#425 = EDGE_LOOP ( 'NONE', ( #5519, #4503, #7362, #1544 ) ) ;
#426 = DIRECTION ( 'NONE',  ( 6.123233995736766036E-17, -1.000000000000000000, 0.000000000000000000 ) ) ;
#427 = CARTESIAN_POINT ( 'NONE',  ( 357.0000000000000000, -4.999999999999998224, 145.0000000000000284 ) ) ;
#428 = VERTEX_POINT ( 'NONE', #5200 ) ;
#429 = ORIENTED_EDGE ( 'NONE', *, *, #1847, .T. ) ;
#430 = LINE ( 'NONE', #3656, #7408 ) ;
#431 = DIRECTION ( 'NONE',  ( -1.734723475976807341E-16, 1.000000000000000000, 0.000000000000000000 ) ) ;
#432 = B_SPLINE_CURVE_WITH_KNOTS ( 'NONE', 3,
 ( #1179, #5739, #3008, #8415, #2453 ),
 .UNSPECIFIED., .F., .F.,
 ( 4, 1, 4 ),
 ( 5.640274452250024914E-20, 0.002309401076758505356, 0.004618802153517010713 ),
 .UNSPECIFIED. ) ;
#433 = DIRECTION ( 'NONE',  ( 0.000000000000000000, 0.000000000000000000, 1.000000000000000000 ) ) ;
#434 =( GEOMETRIC_REPRESENTATION_CONTEXT ( 3 ) GLOBAL_UNCERTAINTY_ASSIGNED_CONTEXT ( ( #457 ) ) GLOBAL_UNIT_ASSIGNED_CONTEXT ( ( #1840, #2417, #5746 ) ) REPRESENTATION_CONTEXT ( 'NONE', 'WORKASPACE' ) );
#435 = CARTESIAN_POINT ( 'NONE',  ( 0.000000000000000000, 0.000000000000000000, 7.000000000000006217 ) ) ;
#436 = EDGE_LOOP ( 'NONE', ( #8463, #5581, #6802, #4042 ) ) ;
#437 = VERTEX_POINT ( 'NONE', #5072 ) ;
#438 = DIRECTION ( 'NONE',  ( -1.000000000000000000, 0.000000000000000000, -0.000000000000000000 ) ) ;
#439 = ADVANCED_FACE ( 'NONE', ( #6505 ), #3771, .T. ) ;
#440 = PRODUCT_DEFINITION_FORMATION_WITH_SPECIFIED_SOURCE ( 'ANY', '', #7953, .NOT_KNOWN. ) ;
#441 = CONICAL_SURFACE ( 'NONE', #1976, 4.000000000000000000, 0.8911886515913786111 ) ;
#442 = EDGE_CURVE ( 'NONE', #5816, #1280, #2302, .T. ) ;
#443 = CARTESIAN_POINT ( 'NONE',  ( -5.000000000000001776, 5.000000000000001776, -36.00000000000000000 ) ) ;
#444 = FACE_OUTER_BOUND ( 'NONE', #8384, .T. ) ;
#445 = EDGE_CURVE ( 'NONE', #1439, #7609, #7238, .T. ) ;
#446 = DIRECTION ( 'NONE',  ( 0.000000000000000000, 0.000000000000000000, 1.000000000000000000 ) ) ;
#447 =( NAMED_UNIT ( * ) SI_UNIT ( $, .STERADIAN. ) SOLID_ANGLE_UNIT ( ) );
#448 = ORIENTED_EDGE ( 'NONE', *, *, #1374, .T. ) ;
#449 = VECTOR ( 'NONE', #5880, 1000.000000000000000 ) ;
#450 = EDGE_CURVE ( 'NONE', #2803, #5343, #1779, .T. ) ;
#451 = FILL_AREA_STYLE_COLOUR ( '', #8108 ) ;
#452 = DIRECTION ( 'NONE',  ( 0.000000000000000000, 0.000000000000000000, 1.000000000000000000 ) ) ;
#453 = AXIS2_PLACEMENT_3D ( 'NONE', #5882, #3158, #8554 ) ;
#454 = CARTESIAN_POINT ( 'NONE',  ( 2.500000000000000000, 2.500728763858895382E-16, -2.041999999999999815 ) ) ;
#455 = CARTESIAN_POINT ( 'NONE',  ( 2.500000000000000000, -1.178949249685213863, 2.042000000000002924 ) ) ;
#456 = VECTOR ( 'NONE', #2169, 1000.000000000000000 ) ;
#457 = UNCERTAINTY_MEASURE_WITH_UNIT (LENGTH_MEASURE( 1.000000000000000082E-05 ), #1840, 'distance_accuracy_value', 'NONE');
#458 = AXIS2_PLACEMENT_3D ( 'NONE', #1269, #3315, #3271 ) ;
#459 = PRESENTATION_LAYER_ASSIGNMENT (  '', '', ( #7272 ) ) ;
#460 = EDGE_LOOP ( 'NONE', ( #4338, #6382, #7676, #2437 ) ) ;
#461 = DIRECTION ( 'NONE',  ( 0.000000000000000000, 1.000000000000000000, 0.000000000000000000 ) ) ;
#462 = COLOUR_RGB ( '',0.8941176470588234615, 0.8941176470588234615, 0.8941176470588234615 ) ;
#463 = ORIENTED_EDGE ( 'NONE', *, *, #2493, .F. ) ;
#464 = DIRECTION ( 'NONE',  ( 0.000000000000000000, 0.000000000000000000, 1.000000000000000000 ) ) ;
#465 = CARTESIAN_POINT ( 'NONE',  ( -4.000000000000000000, 2.309401076758498483, -0.4999999999999927280 ) ) ;
#466 = EDGE_LOOP ( 'NONE', ( #1944, #2418, #2156, #4919 ) ) ;
#467 = EDGE_LOOP ( 'NONE', ( #5929, #7004 ) ) ;
#468 = CARTESIAN_POINT ( 'NONE',  ( -4.999999999999998224, 134.9989999999999952, 25.00000000000000000 ) ) ;
#469 = CIRCLE ( 'NONE', #5320, 2.649999999999985700 ) ;
#470 = LINE ( 'NONE', #7746, #7853 ) ;
#471 =( GEOMETRIC_REPRESENTATION_CONTEXT ( 3 ) GLOBAL_UNCERTAINTY_ASSIGNED_CONTEXT ( ( #1772 ) ) GLOBAL_UNIT_ASSIGNED_CONTEXT ( ( #1714, #488, #8462 ) ) REPRESENTATION_CONTEXT ( 'NONE', 'WORKASPACE' ) );
#472 = APPLICATION_CONTEXT ( 'automotive_design' ) ;
#473 = CARTESIAN_POINT ( 'NONE',  ( -30.00000000000002842, -20.00000000000000000, 180.0000000000000284 ) ) ;
#474 = ORIENTED_EDGE ( 'NONE', *, *, #4612, .F. ) ;
#475 = AXIS2_PLACEMENT_3D ( 'NONE', #136, #7508, #2159 ) ;
#476 = DIRECTION ( 'NONE',  ( -8.995820158514005140E-17, 1.000000000000000000, 2.850801139805002942E-16 ) ) ;
#477 = CARTESIAN_POINT ( 'NONE',  ( -20.00000000000000000, 140.0000000000000000, 4.999999999999997335 ) ) ;
#478 = VERTEX_POINT ( 'NONE', #1205 ) ;
#479 = VERTEX_POINT ( 'NONE', #7117 ) ;
#480 = ADVANCED_FACE ( 'NONE', ( #7780 ), #3861, .T. ) ;
#481 = CARTESIAN_POINT ( 'NONE',  ( -10.00000000000000000, 1.224646799147353256E-15, -115.0000000000000000 ) ) ;
#482 = ADVANCED_FACE ( 'NONE', ( #3818 ), #1820, .F. ) ;
#483 = CARTESIAN_POINT ( 'NONE',  ( 2.500000000000000000, 0.000000000000000000, 0.000000000000000000 ) ) ;
#484 = ADVANCED_FACE ( 'NONE', ( #5765 ), #2597, .F. ) ;
#485 = LINE ( 'NONE', #389, #5908 ) ;
#486 = FACE_OUTER_BOUND ( 'NONE', #2041, .T. ) ;
#487 = ORIENTED_EDGE ( 'NONE', *, *, #5222, .T. ) ;
#488 =( NAMED_UNIT ( * ) PLANE_ANGLE_UNIT ( ) SI_UNIT ( $, .RADIAN. ) );
#489 = VERTEX_POINT ( 'NONE', #588 ) ;
#490 = CARTESIAN_POINT ( 'NONE',  ( -5.000000000000001776, 5.000000000000001776, 148.0000000000000284 ) ) ;
#491 = EDGE_CURVE ( 'NONE', #1367, #1428, #5842, .T. ) ;
#492 = FACE_BOUND ( 'NONE', #3080, .T. ) ;
#493 = DIRECTION ( 'NONE',  ( -0.000000000000000000, -0.000000000000000000, 1.000000000000000000 ) ) ;
#494 = DIRECTION ( 'NONE',  ( 0.000000000000000000, 1.000000000000000000, -1.471414886128461471E-15 ) ) ;
#495 = CARTESIAN_POINT ( 'NONE',  ( 136.6666666666666288, -14.99999999999999822, 162.5000000000000853 ) ) ;
#496 = CARTESIAN_POINT ( 'NONE',  ( -5.000000000000001776, 5.000000000000001776, -0.9999999999999940048 ) ) ;
#497 = CIRCLE ( 'NONE', #1612, 10.00000000000000000 ) ;
#498 = FACE_BOUND ( 'NONE', #7702, .T. ) ;
#499 = VECTOR ( 'NONE', #1824, 1000.000000000000000 ) ;
#500 = DIRECTION ( 'NONE',  ( 0.000000000000000000, 0.000000000000000000, 1.000000000000000000 ) ) ;
#501 = ADVANCED_FACE ( 'NONE', ( #3948 ), #5118, .F. ) ;
#502 = CYLINDRICAL_SURFACE ( 'NONE', #5643, 2.500000000000000444 ) ;
#503 = AXIS2_PLACEMENT_3D ( 'NONE', #3389, #7471, #6027 ) ;
#504 = ORIENTED_EDGE ( 'NONE', *, *, #6187, .T. ) ;
#505 = FACE_OUTER_BOUND ( 'NONE', #2039, .T. ) ;
#506 = EDGE_LOOP ( 'NONE', ( #6682, #4119, #1543, #7518 ) ) ;
#507 = DIRECTION ( 'NONE',  ( 1.734723475976806848E-16, -1.000000000000000000, -0.000000000000000000 ) ) ;
#508 = EDGE_CURVE ( 'NONE', #7885, #3408, #1188, .T. ) ;
#509 = CARTESIAN_POINT ( 'NONE',  ( 0.000000000000000000, 0.000000000000000000, 148.0000000000000284 ) ) ;
#510 = PRESENTATION_LAYER_ASSIGNMENT (  '', '', ( #3293 ) ) ;
#511 = AXIS2_PLACEMENT_3D ( 'NONE', #6789, #836, #2326 ) ;
#512 = ADVANCED_FACE ( 'NONE', ( #5794, #3887 ), #6531, .T. ) ;
#513 = CARTESIAN_POINT ( 'NONE',  ( 24.55500000000002103, 0.000000000000000000, 0.000000000000000000 ) ) ;
#514 = ORIENTED_EDGE ( 'NONE', *, *, #6408, .T. ) ;
#515 = CARTESIAN_POINT ( 'NONE',  ( 0.000000000000000000, 0.000000000000000000, -191.5685424949238325 ) ) ;
#516 = CIRCLE ( 'NONE', #3995, 2.649999999999985700 ) ;
#517 = VECTOR ( 'NONE', #7391, 1000.000000000000000 ) ;
#518 = DIRECTION ( 'NONE',  ( 0.000000000000000000, 1.000000000000000000, 0.000000000000000000 ) ) ;
#519 = CARTESIAN_POINT ( 'NONE',  ( 5.000000000000000000, 5.000000000000000000, -143.0000000000000284 ) ) ;
#520 = EDGE_LOOP ( 'NONE', ( #4607, #2361, #8228, #5907 ) ) ;
#521 = ORIENTED_EDGE ( 'NONE', *, *, #2052, .T. ) ;
#522 = CARTESIAN_POINT ( 'NONE',  ( 444.9999999999999432, -4.999999999999998224, 139.9990000000000236 ) ) ;
#523 = DIRECTION ( 'NONE',  ( -0.000000000000000000, -0.000000000000000000, -1.000000000000000000 ) ) ;
#524 = CYLINDRICAL_SURFACE ( 'NONE', #783, 2.649999999999985700 ) ;
#525 = EDGE_CURVE ( 'NONE', #989, #7549, #930, .T. ) ;
#526 = DIRECTION ( 'NONE',  ( -1.734723475976806848E-16, 1.000000000000000000, 0.000000000000000000 ) ) ;
#527 = ORIENTED_EDGE ( 'NONE', *, *, #5024, .F. ) ;
#528 = SHAPE_REPRESENTATION_RELATIONSHIP ( 'NONE' , 'NONE' ,  #2984, #2539 ) ;
#529 = EDGE_LOOP ( 'NONE', ( #8443, #6852, #7945 ) ) ;
#530 = VERTEX_POINT ( 'NONE', #8502 ) ;
#531 = DIRECTION ( 'NONE',  ( -1.000000000000000000, 1.734723475976806848E-16, -0.000000000000000000 ) ) ;
#532 = FACE_BOUND ( 'NONE', #1186, .T. ) ;
#533 = FACE_OUTER_BOUND ( 'NONE', #460, .T. ) ;
#534 = DIRECTION ( 'NONE',  ( 0.000000000000000000, 1.000000000000000000, 0.000000000000000000 ) ) ;
#535 = CONICAL_SURFACE ( 'NONE', #1230, 5.560781378645573980, 1.221730476396046816 ) ;
#536 = DIRECTION ( 'NONE',  ( 0.000000000000000000, 0.000000000000000000, -1.000000000000000000 ) ) ;
#537 = CYLINDRICAL_SURFACE ( 'NONE', #7711, 10.00000000000000000 ) ;
#538 = CARTESIAN_POINT ( 'NONE',  ( -5.000000000000000000, -5.000000000000000000, 148.0000000000000284 ) ) ;
#539 = AXIS2_PLACEMENT_3D ( 'NONE', #8100, #4108, #804 ) ;
#540 = FACE_OUTER_BOUND ( 'NONE', #466, .T. ) ;
#541 = CARTESIAN_POINT ( 'NONE',  ( 136.6666666666666288, -20.00000000000000000, 159.8500000000001080 ) ) ;
#542 = VERTEX_POINT ( 'NONE', #2423 ) ;
#543 = DIRECTION ( 'NONE',  ( -1.734723475976806848E-16, 1.000000000000000000, 0.000000000000000000 ) ) ;
#544 = ORIENTED_EDGE ( 'NONE', *, *, #5815, .F. ) ;
#545 = CARTESIAN_POINT ( 'NONE',  ( 347.0000000000000000, 5.000000000000001776, 145.0000000000000284 ) ) ;
#546 = AXIS2_PLACEMENT_3D ( 'NONE', #7851, #3806, #1061 ) ;
#547 = DIRECTION ( 'NONE',  ( 0.000000000000000000, -1.000000000000000000, 0.000000000000000000 ) ) ;
#548 = ADVANCED_FACE ( 'NONE', ( #2464 ), #6493, .F. ) ;
#549 = CARTESIAN_POINT ( 'NONE',  ( 5.000000000000000000, -5.000000000000000000, 140.0000000000000000 ) ) ;
#550 = CONICAL_SURFACE ( 'NONE', #6527, 2.059999999999998721, 0.9599310885968738161 ) ;
#551 = EDGE_CURVE ( 'NONE', #2756, #4735, #3107, .T. ) ;
#552 = ORIENTED_EDGE ( 'NONE', *, *, #6640, .T. ) ;
#553 = CARTESIAN_POINT ( 'NONE',  ( 259.0000000000000000, -4.999999999999998224, 140.0000000000000000 ) ) ;
#554 = APPLICATION_PROTOCOL_DEFINITION ( 'draft international standard', 'automotive_design', 1998, #7764 ) ;
#555 = DIRECTION ( 'NONE',  ( 0.000000000000000000, 1.000000000000000000, 0.000000000000000000 ) ) ;
#556 = ORIENTED_EDGE ( 'NONE', *, *, #5443, .T. ) ;
#557 = ADVANCED_FACE ( 'NONE', ( #3066, #4491, #7149, #1189, #3755, #5751, #532, #2545, #5707, #1264, #492, #1890 ), #402, .F. ) ;
#558 = ORIENTED_EDGE ( 'NONE', *, *, #1197, .T. ) ;
#559 = CARTESIAN_POINT ( 'NONE',  ( -5.000000000000001776, 5.000000000000001776, 140.0000000000000000 ) ) ;
#560 = CARTESIAN_POINT ( 'NONE',  ( 5.000000000000000000, -5.000000000000000000, 148.0000000000000284 ) ) ;
#561 = PLANE ( 'NONE',  #4523 ) ;
#562 = FACE_OUTER_BOUND ( 'NONE', #280, .T. ) ;
#563 = VERTEX_POINT ( 'NONE', #6362 ) ;
#564 =( NAMED_UNIT ( * ) PLANE_ANGLE_UNIT ( ) SI_UNIT ( $, .RADIAN. ) );
#565 = EDGE_LOOP ( 'NONE', ( #768, #2358, #3387, #1842 ) ) ;
#566 = LINE ( 'NONE', #5394, #3941 ) ;
#567 = ADVANCED_FACE ( 'NONE', ( #8467, #3192 ), #5186, .T. ) ;
#568 = AXIS2_PLACEMENT_3D ( 'NONE', #1128, #1791, #1045 ) ;
#569 = CARTESIAN_POINT ( 'NONE',  ( 0.000000000000000000, 0.000000000000000000, 140.0000000000000000 ) ) ;
#570 = DIRECTION ( 'NONE',  ( -0.000000000000000000, -0.000000000000000000, -1.000000000000000000 ) ) ;
#571 = DIRECTION ( 'NONE',  ( -0.000000000000000000, -0.000000000000000000, 1.000000000000000000 ) ) ;
#572 = CARTESIAN_POINT ( 'NONE',  ( 0.000000000000000000, 0.000000000000000000, -27.99999999999999645 ) ) ;
#573 = LINE ( 'NONE', #1972, #5544 ) ;
#574 = PRODUCT_DEFINITION_SHAPE ( 'NONE', 'NONE',  #5006 ) ;
#575 = CARTESIAN_POINT ( 'NONE',  ( -30.00000000000002842, -20.00000000000000000, 180.0000000000000284 ) ) ;
#576 = LINE ( 'NONE', #1273, #5469 ) ;
#577 = EDGE_CURVE ( 'NONE', #133, #2563, #1209, .T. ) ;
#578 = EDGE_CURVE ( 'NONE', #4191, #4735, #5829, .T. ) ;
#579 = CARTESIAN_POINT ( 'NONE',  ( 4.000000000000000000, 0.3987449864460005378, -0.01220643443059817035 ) ) ;
#580 = EDGE_CURVE ( 'NONE', #8517, #6781, #7849, .T. ) ;
#581=STYLED_ITEM('',(#8650),#4654);
#582 = LINE ( 'NONE', #6341, #7776 ) ;
#583 = CARTESIAN_POINT ( 'NONE',  ( 219.9999999999999716, -20.00000000000000000, 162.5000000000000853 ) ) ;
#584 =( BOUNDED_SURFACE ( )  B_SPLINE_SURFACE ( 3, 2, ( 
 ( #4413, #7770, #1723 ),
 ( #3024, #1021, #1677 ),
 ( #7641, #1106, #4324 ),
 ( #3677, #4282, #6930 ),
 ( #7022, #6323, #5671 ),
 ( #8340, #2381, #3759 ) ),
 .UNSPECIFIED., .F., .F., .T. ) 
 B_SPLINE_SURFACE_WITH_KNOTS ( ( 4, 2, 4 ),
 ( 3, 3 ),
 ( 0.02027752710269158445, 0.02273781595091097299, 0.02519810479913036153 ),
 ( 0.000000000000000000, 1.000000000000000000 ),
 .UNSPECIFIED. ) 
 GEOMETRIC_REPRESENTATION_ITEM ( )  RATIONAL_B_SPLINE_SURFACE ( (
 ( 1.000000000000000000, 0.8047781431712808242, 1.000000000000000000),
 ( 1.000000000000000000, 0.8123773247083928561, 1.000000000000000000),
 ( 1.000000000000000000, 0.8190670192154906326, 1.000000000000000000),
 ( 1.000000000000000000, 0.8192353552912178261, 1.000000000000000000),
 ( 1.000000000000000000, 0.8126132098226825917, 1.000000000000000000),
 ( 1.000000000000000000, 0.8047712465856394770, 1.000000000000000000) ) ) 
 REPRESENTATION_ITEM ( '' )  SURFACE ( )  );
#585 = ORIENTED_EDGE ( 'NONE', *, *, #6271, .T. ) ;
#586 =( NAMED_UNIT ( * ) SI_UNIT ( $, .STERADIAN. ) SOLID_ANGLE_UNIT ( ) );
#587 = AXIS2_PLACEMENT_3D ( 'NONE', #8475, #2553, #2629 ) ;
#588 = CARTESIAN_POINT ( 'NONE',  ( 10.00000000000000000, 0.000000000000000000, -63.99999999999997158 ) ) ;
#589 = ITEM_DEFINED_TRANSFORMATION ( 'NONE', 'NONE', #1558,  #594 ) ;
#590 = VERTEX_POINT ( 'NONE', #1227 ) ;
#591 = DIRECTION ( 'NONE',  ( -1.000000000000000000, -0.000000000000000000, -0.000000000000000000 ) ) ;
#592 = AXIS2_PLACEMENT_3D ( 'NONE', #1582, #4234, #309 ) ;
#593 = CARTESIAN_POINT ( 'NONE',  ( 5.000000000000000000, 135.0000000000000000, 25.00000000000000000 ) ) ;
#594 = AXIS2_PLACEMENT_3D ( 'NONE', #3123, #464, #5764 ) ;
#595 = FACE_OUTER_BOUND ( 'NONE', #7513, .T. ) ;
#596 = VERTEX_POINT ( 'NONE', #3235 ) ;
#597 = ADVANCED_FACE ( 'NONE', ( #5875 ), #3156, .F. ) ;
#598 = AXIS2_PLACEMENT_3D ( 'NONE', #5344, #7214, #4044 ) ;
#599 = CARTESIAN_POINT ( 'NONE',  ( -5.000000000000000000, -5.000000000000000000, 140.0000000000000000 ) ) ;
#600 = SHAPE_DEFINITION_REPRESENTATION ( #5299, #7686 ) ;
#601 = FACE_BOUND ( 'NONE', #6016, .T. ) ;
#602 = ORIENTED_EDGE ( 'NONE', *, *, #5769, .F. ) ;
#603 = VECTOR ( 'NONE', #2035, 1000.000000000000000 ) ;
#604 = ORIENTED_EDGE ( 'NONE', *, *, #7855, .F. ) ;
#605 = CARTESIAN_POINT ( 'NONE',  ( 5.000000000000000000, -5.000000000000000000, -143.0000000000000284 ) ) ;
#606 = FACE_OUTER_BOUND ( 'NONE', #8585, .T. ) ;
#607 = EDGE_CURVE ( 'NONE', #3740, #2174, #5920, .T. ) ;
#608 = AXIS2_PLACEMENT_3D ( 'NONE', #7647, #6285, #365 ) ;
#609 = FACE_OUTER_BOUND ( 'NONE', #8309, .T. ) ;
#610 = DIRECTION ( 'NONE',  ( 0.000000000000000000, -1.000000000000000000, 0.000000000000000000 ) ) ;
#611 = ORIENTED_EDGE ( 'NONE', *, *, #6429, .F. ) ;
#612 = AXIS2_PLACEMENT_3D ( 'NONE', #910, #7570, #1605 ) ;
#613 = SURFACE_STYLE_USAGE ( .BOTH. , #5951 ) ;
#614 = EDGE_LOOP ( 'NONE', ( #2947, #918 ) ) ;
#615 = CARTESIAN_POINT ( 'NONE',  ( 2.500000000000000000, 0.000000000000000000, 2.041999999999999815 ) ) ;
#616 = VECTOR ( 'NONE', #2532, 1000.000000000000000 ) ;
#617 = DIRECTION ( 'NONE',  ( 0.000000000000000000, -1.000000000000000000, 0.000000000000000000 ) ) ;
#618 = DIRECTION ( 'NONE',  ( -1.734723475976806848E-16, 1.000000000000000000, 0.000000000000000000 ) ) ;
#619 = ORIENTED_EDGE ( 'NONE', *, *, #306, .T. ) ;
#620 = DIRECTION ( 'NONE',  ( 0.000000000000000000, 0.000000000000000000, -1.000000000000000000 ) ) ;
#621 = CARTESIAN_POINT ( 'NONE',  ( -10.00000000000000000, 1.224646799147353059E-15, -27.99999999999999645 ) ) ;
#622 = DIRECTION ( 'NONE',  ( -1.000000000000000000, -0.000000000000000000, -0.000000000000000000 ) ) ;
#623 = CARTESIAN_POINT ( 'NONE',  ( 4.154306624731035846, -2.398490048085128556, -3.721999068284417955 ) ) ;
#624 = FACE_OUTER_BOUND ( 'NONE', #6447, .T. ) ;
#625 = LINE ( 'NONE', #2721, #7491 ) ;
#626 = DIRECTION ( 'NONE',  ( 0.000000000000000000, 0.000000000000000000, 1.000000000000000000 ) ) ;
#627 = EDGE_CURVE ( 'NONE', #5001, #8500, #3020, .T. ) ;
#628 = VERTEX_POINT ( 'NONE', #4013 ) ;
#629 = ADVANCED_FACE ( 'NONE', ( #82 ), #6046, .F. ) ;
#630 = SURFACE_STYLE_FILL_AREA ( #7114 ) ;
#631 = ORIENTED_EDGE ( 'NONE', *, *, #5473, .T. ) ;
#632 = AXIS2_PLACEMENT_3D ( 'NONE', #468, #1079, #5768 ) ;
#633 = ORIENTED_EDGE ( 'NONE', *, *, #2383, .T. ) ;
#634 =( REPRESENTATION_RELATIONSHIP ('NONE','NONE', #3312, #2707 ) REPRESENTATION_RELATIONSHIP_WITH_TRANSFORMATION ( #4084 )SHAPE_REPRESENTATION_RELATIONSHIP( ) );
#635 = CARTESIAN_POINT ( 'NONE',  ( 88.00000000000000000, -20.00000000000000000, -121.8314250403154659 ) ) ;
#636 = LINE ( 'NONE', #12, #7410 ) ;
#637 = PRODUCT_DEFINITION_CONTEXT ( 'detailed design', #7921, 'design' ) ;
#638 = SHAPE_REPRESENTATION ( 'roller axis assy_r4', ( #594 ), #1694 ) ;
#639 = CARTESIAN_POINT ( 'NONE',  ( -6.259644161404860030E-16, -4.618802153517027165, -3.433295621305388234 ) ) ;
#640 = ORIENTED_EDGE ( 'NONE', *, *, #7790, .T. ) ;
#641 = CARTESIAN_POINT ( 'NONE',  ( 444.9999999999999432, 5.000000000000000000, 145.0000000000000284 ) ) ;
#642 = SHAPE_DEFINITION_REPRESENTATION ( #4132, #7424 ) ;
#643 = ADVANCED_FACE ( 'NONE', ( #2664 ), #5353, .F. ) ;
#644 = DIRECTION ( 'NONE',  ( 1.000000000000000000, 1.734723475976806848E-16, 0.000000000000000000 ) ) ;
#645 = ORIENTED_EDGE ( 'NONE', *, *, #8589, .F. ) ;
#646 = ORIENTED_EDGE ( 'NONE', *, *, #3675, .F. ) ;
#647 = VECTOR ( 'NONE', #2635, 1000.000000000000000 ) ;
#649 = VECTOR ( 'NONE', #3687, 1000.000000000000000 ) ;
#648 = DIRECTION ( 'NONE',  ( -1.000000000000000000, 0.000000000000000000, 0.000000000000000000 ) ) ;
#650 = CARTESIAN_POINT ( 'NONE',  ( 82.99999999999998579, -4.999999999999998224, 139.9990000000000236 ) ) ;
#651=STYLED_ITEM('',(#8678),#2244);
#652 = CARTESIAN_POINT ( 'NONE',  ( 0.6507732100473444525, -4.243078065514795050, -0.2236248678334952777 ) ) ;
#653 = CIRCLE ( 'NONE', #5515, 5.560781378645573980 ) ;
#654 = PRODUCT ( 'roller axis assy_r5', 'roller axis assy_r5', '', ( #7013 ) ) ;
#655 = FACE_OUTER_BOUND ( 'NONE', #4653, .T. ) ;
#656 = EDGE_LOOP ( 'NONE', ( #7632, #980, #7793, #6433 ) ) ;
#657 =( LENGTH_UNIT ( ) NAMED_UNIT ( * ) SI_UNIT ( .MILLI., .METRE. ) );
#658 = EDGE_LOOP ( 'NONE', ( #8272, #6605, #4968, #328 ) ) ;
#659 = CARTESIAN_POINT ( 'NONE',  ( 5.000000000000000000, -5.000000000000000000, 7.000000000000006217 ) ) ;
#660 = DIRECTION ( 'NONE',  ( 1.000000000000000000, 0.000000000000000000, 0.000000000000000000 ) ) ;
#661 = EDGE_CURVE ( 'NONE', #7356, #2201, #5955, .T. ) ;
#662 = DIRECTION ( 'NONE',  ( -0.000000000000000000, 1.000000000000000000, -0.000000000000000000 ) ) ;
#663 = ORIENTED_EDGE ( 'NONE', *, *, #3639, .T. ) ;
#664 = DIRECTION ( 'NONE',  ( 0.000000000000000000, 0.000000000000000000, -1.000000000000000000 ) ) ;
#665 =( LENGTH_UNIT ( ) NAMED_UNIT ( * ) SI_UNIT ( .MILLI., .METRE. ) );
#666 = EDGE_CURVE ( 'NONE', #242, #2803, #2187, .T. ) ;
#667 = CARTESIAN_POINT ( 'NONE',  ( 434.9999999999999432, 5.000000000000001776, 140.0000000000000000 ) ) ;
#668 = EDGE_CURVE ( 'NONE', #3213, #3699, #4707, .T. ) ;
#669 = DIRECTION ( 'NONE',  ( 1.734723475976806848E-16, -1.000000000000000000, -0.000000000000000000 ) ) ;
#670 = CARTESIAN_POINT ( 'NONE',  ( -2.000000000000006661, 3.464101615137750834, 0.000000000000000000 ) ) ;
#671 = DIRECTION ( 'NONE',  ( -1.000000000000000000, -0.000000000000000000, -0.000000000000000000 ) ) ;
#672 = CARTESIAN_POINT ( 'NONE',  ( 10.00000000000000000, 0.000000000000000000, 140.0000000000000000 ) ) ;
#673 = DIRECTION ( 'NONE',  ( -0.000000000000000000, -0.000000000000000000, 1.000000000000000000 ) ) ;
#674 = AXIS2_PLACEMENT_3D ( 'NONE', #6837, #7536, #1532 ) ;
#675 = ORIENTED_EDGE ( 'NONE', *, *, #4538, .T. ) ;
#676 = ORIENTED_EDGE ( 'NONE', *, *, #5459, .T. ) ;
#677 = ITEM_DEFINED_TRANSFORMATION ( 'NONE', 'NONE', #7952,  #594 ) ;
#678 = VERTEX_POINT ( 'NONE', #39 ) ;
#679 = CARTESIAN_POINT ( 'NONE',  ( 386.6666666666666288, -20.00000000000000000, 159.8500000000001080 ) ) ;
#680 = LINE ( 'NONE', #6020, #603 ) ;
#681 = EDGE_CURVE ( 'NONE', #54, #5626, #751, .T. ) ;
#682 = VECTOR ( 'NONE', #1278, 1000.000000000000000 ) ;
#683 = CARTESIAN_POINT ( 'NONE',  ( 5.000000000000000000, 5.000000000000000000, -105.9999999999999858 ) ) ;
#684 = ORIENTED_EDGE ( 'NONE', *, *, #4886, .F. ) ;
#685 = DIRECTION ( 'NONE',  ( -1.000000000000000000, 0.000000000000000000, 0.000000000000000000 ) ) ;
#686 = FACE_BOUND ( 'NONE', #6675, .T. ) ;
#687 = AXIS2_PLACEMENT_3D ( 'NONE', #1011, #5618, #4883 ) ;
#688 = CARTESIAN_POINT ( 'NONE',  ( -1.828356344711647319, -3.563200125723192002, -1.076197711133951296E-14 ) ) ;
#689 = EDGE_LOOP ( 'NONE', ( #272, #8189, #1322, #1809 ) ) ;
#690 = ORIENTED_EDGE ( 'NONE', *, *, #334, .F. ) ;
#691 = CARTESIAN_POINT ( 'NONE',  ( 259.0000000000000000, -4.999999999999998224, 145.0000000000000284 ) ) ;
#692 = DIRECTION ( 'NONE',  ( 0.000000000000000000, 0.000000000000000000, 1.000000000000000000 ) ) ;
#693 = VECTOR ( 'NONE', #5102, 1000.000000000000000 ) ;
#694 = DIRECTION ( 'NONE',  ( 1.000000000000000000, 1.734723475976807587E-16, 0.000000000000000000 ) ) ;
#695 = DIRECTION ( 'NONE',  ( 0.000000000000000000, 0.000000000000000000, 1.000000000000000000 ) ) ;
#696 = EDGE_LOOP ( 'NONE', ( #1832, #514, #6791, #6324 ) ) ;
#697 =( NAMED_UNIT ( * ) SI_UNIT ( $, .STERADIAN. ) SOLID_ANGLE_UNIT ( ) );
#698 = ORIENTED_EDGE ( 'NONE', *, *, #7696, .T. ) ;
#699 = DIRECTION ( 'NONE',  ( 0.000000000000000000, 0.000000000000000000, 1.000000000000000000 ) ) ;
#700 = CARTESIAN_POINT ( 'NONE',  ( 5.000000000000000000, 5.000000000000000000, -143.0000000000000284 ) ) ;
#701 = LINE ( 'NONE', #6002, #1786 ) ;
#702 = VERTEX_POINT ( 'NONE', #1004 ) ;
#703 = CARTESIAN_POINT ( 'NONE',  ( -4.154094228333456762, 2.398367420968013253, -3.721909803043220055 ) ) ;
#704 = EDGE_CURVE ( 'NONE', #3882, #5674, #2793, .T. ) ;
#705 = DIRECTION ( 'NONE',  ( 1.000000000000000000, 0.000000000000000000, 0.000000000000000000 ) ) ;
#706 = EDGE_CURVE ( 'NONE', #6409, #7056, #2096, .T. ) ;
#707 = DIRECTION ( 'NONE',  ( -0.000000000000000000, 1.000000000000000000, -0.000000000000000000 ) ) ;
#708 = ADVANCED_FACE ( 'NONE', ( #7273 ), #6614, .F. ) ;
#709 = DIRECTION ( 'NONE',  ( -0.000000000000000000, -0.000000000000000000, 1.000000000000000000 ) ) ;
#710 = ADVANCED_FACE ( 'NONE', ( #8116, #1310 ), #8590, .F. ) ;
#711 = DIRECTION ( 'NONE',  ( -0.000000000000000000, -0.000000000000000000, 1.000000000000000000 ) ) ;
#712 = MECHANICAL_DESIGN_GEOMETRIC_PRESENTATION_REPRESENTATION (  '', ( #6410 ), #7388 ) ;
#713 = ORIENTED_EDGE ( 'NONE', *, *, #3006, .F. ) ;
#714 = SURFACE_STYLE_USAGE ( .BOTH. , #6668 ) ;
#715 = EDGE_LOOP ( 'NONE', ( #5309, #6953, #3557, #6643 ) ) ;
#716 = VERTEX_POINT ( 'NONE', #3406 ) ;
#717 = CARTESIAN_POINT ( 'NONE',  ( 0.000000000000000000, 0.000000000000000000, -5.000000000000000000 ) ) ;
#718 = CARTESIAN_POINT ( 'NONE',  ( 0.6448876103708359731, 4.246476118072354922, -0.2256878752776725616 ) ) ;
#719 = PRODUCT_DEFINITION_FORMATION_WITH_SPECIFIED_SOURCE ( 'ANY', '', #7464, .NOT_KNOWN. ) ;
#720 = PRODUCT_DEFINITION_SHAPE ( 'NONE', 'NONE',  #8610 ) ;
#721 =( GEOMETRIC_REPRESENTATION_CONTEXT ( 3 ) GLOBAL_UNCERTAINTY_ASSIGNED_CONTEXT ( ( #3933 ) ) GLOBAL_UNIT_ASSIGNED_CONTEXT ( ( #6030, #65, #145 ) ) REPRESENTATION_CONTEXT ( 'NONE', 'WORKASPACE' ) );
#722 = EDGE_LOOP ( 'NONE', ( #7433, #7623, #8054, #2319 ) ) ;
#723 = PLANE ( 'NONE',  #213 ) ;
#724 = AXIS2_PLACEMENT_3D ( 'NONE', #6139, #2104, #89 ) ;
#725 = ORIENTED_EDGE ( 'NONE', *, *, #2747, .T. ) ;
#726 = CARTESIAN_POINT ( 'NONE',  ( 20.00000000000000000, 135.0000000000000000, 40.00000000000000000 ) ) ;
#727 = CARTESIAN_POINT ( 'NONE',  ( 5.000000000000000000, -5.000000000000000000, 140.0000000000000000 ) ) ;
#728 = DIRECTION ( 'NONE',  ( -0.4536386087135128031, 0.000000000000000000, -0.8911857341118454290 ) ) ;
#729 = DIRECTION ( 'NONE',  ( -0.000000000000000000, 1.000000000000000000, -0.000000000000000000 ) ) ;
#730 = VERTEX_POINT ( 'NONE', #3974 ) ;
#731 = CIRCLE ( 'NONE', #310, 20.00000000000000000 ) ;
#732 = VERTEX_POINT ( 'NONE', #4102 ) ;
#733 = DIRECTION ( 'NONE',  ( 0.000000000000000000, -1.000000000000000000, 0.000000000000000000 ) ) ;
#734 = DIRECTION ( 'NONE',  ( 1.000000000000000000, 1.734723475976807587E-16, 0.000000000000000000 ) ) ;
#735 = AXIS2_PLACEMENT_3D ( 'NONE', #5336, #5207, #3342 ) ;
#736 = CIRCLE ( 'NONE', #1858, 2.500000000000000888 ) ;
#737 = FACE_OUTER_BOUND ( 'NONE', #3619, .T. ) ;
#738 = DIRECTION ( 'NONE',  ( 1.000000000000000000, 0.000000000000000000, 0.000000000000000000 ) ) ;
#739 = ORIENTED_EDGE ( 'NONE', *, *, #781, .T. ) ;
#740 = VECTOR ( 'NONE', #3211, 1000.000000000000000 ) ;
#741 = PRESENTATION_LAYER_ASSIGNMENT (  '', '', ( #7560 ) ) ;
#742 = ADVANCED_FACE ( 'NONE', ( #3927 ), #2016, .F. ) ;
#743 =( LENGTH_UNIT ( ) NAMED_UNIT ( * ) SI_UNIT ( .MILLI., .METRE. ) );
#744 = DIRECTION ( 'NONE',  ( -1.734723475976806848E-16, 1.000000000000000000, 0.000000000000000000 ) ) ;
#745 = EDGE_CURVE ( 'NONE', #1823, #8068, #1628, .T. ) ;
#746 = ORIENTED_EDGE ( 'NONE', *, *, #4372, .F. ) ;
#747 = DIRECTION ( 'NONE',  ( -0.000000000000000000, -0.000000000000000000, -1.000000000000000000 ) ) ;
#748 = ADVANCED_FACE ( 'NONE', ( #7933 ), #368, .F. ) ;
#749 = VECTOR ( 'NONE', #5021, 1000.000000000000000 ) ;
#750 =( GEOMETRIC_REPRESENTATION_CONTEXT ( 3 ) GLOBAL_UNCERTAINTY_ASSIGNED_CONTEXT ( ( #53 ) ) GLOBAL_UNIT_ASSIGNED_CONTEXT ( ( #4971, #4232, #7588 ) ) REPRESENTATION_CONTEXT ( 'NONE', 'WORKASPACE' ) );
#751 = LINE ( 'NONE', #3447, #4670 ) ;
#752 = FACE_OUTER_BOUND ( 'NONE', #3034, .T. ) ;
#753 = ADVANCED_FACE ( 'NONE', ( #4656 ), #3358, .F. ) ;
#754 = ORIENTED_EDGE ( 'NONE', *, *, #3538, .T. ) ;
#755 = CARTESIAN_POINT ( 'NONE',  ( -5.000000000000000000, -5.000000000000000000, 42.00000000000000711 ) ) ;
#756 = AXIS2_PLACEMENT_3D ( 'NONE', #8216, #4153, #2726 ) ;
#757 = DIRECTION ( 'NONE',  ( -0.000000000000000000, -0.000000000000000000, 1.000000000000000000 ) ) ;
#758 = EDGE_CURVE ( 'NONE', #2389, #2221, #6961, .T. ) ;
#759 = ADVANCED_BREP_SHAPE_REPRESENTATION ( '', ( #7573, #594 ), #750 ) ;
#760 = CARTESIAN_POINT ( 'NONE',  ( -5.000000000000001776, 5.000000000000001776, 148.0000000000000284 ) ) ;
#761 = VECTOR ( 'NONE', #8600, 1000.000000000000000 ) ;
#762 = CARTESIAN_POINT ( 'NONE',  ( 5.000000000000000000, 5.000000000000000000, -143.0000000000000284 ) ) ;
#763 = CARTESIAN_POINT ( 'NONE',  ( -30.00000000000000000, 15.00000000000000000, 145.0000000000000284 ) ) ;
#764 = FACE_OUTER_BOUND ( 'NONE', #6922, .T. ) ;
#765 = VERTEX_POINT ( 'NONE', #923 ) ;
#766 = ORIENTED_EDGE ( 'NONE', *, *, #850, .F. ) ;
#767 = UNCERTAINTY_MEASURE_WITH_UNIT (LENGTH_MEASURE( 1.000000000000000082E-05 ), #3325, 'distance_accuracy_value', 'NONE');
#768 = ORIENTED_EDGE ( 'NONE', *, *, #1199, .F. ) ;
#769 = CARTESIAN_POINT ( 'NONE',  ( 88.00000000000000000, -20.00000000000000000, -119.1814250403154745 ) ) ;
#770 = FACE_OUTER_BOUND ( 'NONE', #6133, .T. ) ;
#771 = VERTEX_POINT ( 'NONE', #3578 ) ;
#772 = CARTESIAN_POINT ( 'NONE',  ( 0.000000000000000000, 0.000000000000000000, 140.0000000000000000 ) ) ;
#773 = ORIENTED_EDGE ( 'NONE', *, *, #4245, .T. ) ;
#774 = CARTESIAN_POINT ( 'NONE',  ( 4.211140560182196957, -2.431303136016555122, -3.745885042887436622 ) ) ;
#775 = CARTESIAN_POINT ( 'NONE',  ( 5.000000000000000000, -5.000000000000000000, 148.0000000000000284 ) ) ;
#776 = EDGE_CURVE ( 'NONE', #1841, #8324, #2475, .T. ) ;
#777 = FILL_AREA_STYLE_COLOUR ( '', #6834 ) ;
#778 = ORIENTED_EDGE ( 'NONE', *, *, #8445, .T. ) ;
#779 = ORIENTED_EDGE ( 'NONE', *, *, #3163, .F. ) ;
#780 = CARTESIAN_POINT ( 'NONE',  ( 434.9999999999999432, -4.999999999999998224, 145.0000000000000284 ) ) ;
#781 = EDGE_CURVE ( 'NONE', #4350, #1013, #7584, .T. ) ;
#782 = CARTESIAN_POINT ( 'NONE',  ( 1.411581201560190495E-15, 4.862606272033091592, -3.745885042887436622 ) ) ;
#783 = AXIS2_PLACEMENT_3D ( 'NONE', #5091, #5820, #5173 ) ;
#784 = CARTESIAN_POINT ( 'NONE',  ( 2.000000000000005329, -3.464101615137751722, 0.000000000000000000 ) ) ;
#785 = DIRECTION ( 'NONE',  ( 0.000000000000000000, 1.000000000000000000, 0.000000000000000000 ) ) ;
#786 = ORIENTED_EDGE ( 'NONE', *, *, #578, .T. ) ;
#787 = VECTOR ( 'NONE', #230, 1000.000000000000000 ) ;
#788 = SURFACE_STYLE_USAGE ( .BOTH. , #206 ) ;
#789 = DIRECTION ( 'NONE',  ( 0.000000000000000000, 0.000000000000000000, -1.000000000000000000 ) ) ;
#790 = ORIENTED_EDGE ( 'NONE', *, *, #3133, .F. ) ;
#791 = EDGE_LOOP ( 'NONE', ( #358, #3547, #5822, #6456, #2085, #271 ) ) ;
#792 = DIRECTION ( 'NONE',  ( 1.000000000000000000, 0.000000000000000000, 0.000000000000000000 ) ) ;
#793 = AXIS2_PLACEMENT_3D ( 'NONE', #3331, #7235, #6502 ) ;
#794 = EDGE_CURVE ( 'NONE', #7699, #1878, #8026, .T. ) ;
#795 = VECTOR ( 'NONE', #4140, 1000.000000000000000 ) ;
#796 = DIRECTION ( 'NONE',  ( -1.000000000000000000, 0.000000000000000000, 0.000000000000000000 ) ) ;
#797 = CARTESIAN_POINT ( 'NONE',  ( 0.000000000000000000, 0.000000000000000000, 4.000000000000000000 ) ) ;
#798 = VERTEX_POINT ( 'NONE', #5567 ) ;
#799 = CARTESIAN_POINT ( 'NONE',  ( -10.00000000000000000, 1.224646799147353256E-15, 120.0000000000000284 ) ) ;
#800 = FACE_OUTER_BOUND ( 'NONE', #286, .T. ) ;
#801 = CARTESIAN_POINT ( 'NONE',  ( 0.000000000000000000, 0.000000000000000000, 140.0000000000000000 ) ) ;
#802 =( REPRESENTATION_RELATIONSHIP ('NONE','NONE', #3312, #638 ) REPRESENTATION_RELATIONSHIP_WITH_TRANSFORMATION ( #5682 )SHAPE_REPRESENTATION_RELATIONSHIP( ) );
#803 = FACE_OUTER_BOUND ( 'NONE', #6038, .T. ) ;
#804 = DIRECTION ( 'NONE',  ( 0.000000000000000000, 0.000000000000000000, 1.000000000000000000 ) ) ;
#805 = DIRECTION ( 'NONE',  ( 0.000000000000000000, 0.000000000000000000, -1.000000000000000000 ) ) ;
#806 = VERTEX_POINT ( 'NONE', #6265 ) ;
#807 = VERTEX_POINT ( 'NONE', #1006 ) ;
#808 = VERTEX_POINT ( 'NONE', #2280 ) ;
#809 = DIRECTION ( 'NONE',  ( 0.000000000000000000, 0.000000000000000000, 1.000000000000000000 ) ) ;
#810 = CARTESIAN_POINT ( 'NONE',  ( -5.000000000000000000, -5.000000000000000000, 148.0000000000000284 ) ) ;
#811 = EDGE_LOOP ( 'NONE', ( #463, #5711, #6252, #6400 ) ) ;
#812 = DIRECTION ( 'NONE',  ( -1.000000000000000000, 0.000000000000000000, 0.000000000000000000 ) ) ;
#813 = ORIENTED_EDGE ( 'NONE', *, *, #6403, .F. ) ;
#814 = FACE_OUTER_BOUND ( 'NONE', #467, .T. ) ;
#815 = DIRECTION ( 'NONE',  ( -1.000000000000000000, 0.000000000000000000, -0.000000000000000000 ) ) ;
#816 = SHAPE_DEFINITION_REPRESENTATION ( #8175, #1533 ) ;
#817 = SURFACE_SIDE_STYLE ('',( #7474 ) ) ;
#818 = EDGE_LOOP ( 'NONE', ( #7207, #3911, #376, #7380 ) ) ;
#819 = VERTEX_POINT ( 'NONE', #4271 ) ;
#820 = DIRECTION ( 'NONE',  ( -0.000000000000000000, -0.000000000000000000, 1.000000000000000000 ) ) ;
#821 = CIRCLE ( 'NONE', #5944, 2.649999999999985700 ) ;
#822 = DIRECTION ( 'NONE',  ( 0.000000000000000000, 0.000000000000000000, 1.000000000000000000 ) ) ;
#823 = EDGE_CURVE ( 'NONE', #1959, #4658, #1487, .T. ) ;
#824 = ADVANCED_FACE ( 'NONE', ( #303, #3493 ), #7627, .T. ) ;
#825 = DIRECTION ( 'NONE',  ( -0.000000000000000000, 1.000000000000000000, -0.000000000000000000 ) ) ;
#826 = AXIS2_PLACEMENT_3D ( 'NONE', #2999, #3245, #8556 ) ;
#827 = CARTESIAN_POINT ( 'NONE',  ( -5.000000000000000000, -5.000000000000000000, -71.99999999999998579 ) ) ;
#828 = ORIENTED_EDGE ( 'NONE', *, *, #3798, .T. ) ;
#830 = EDGE_CURVE ( 'NONE', #5455, #1089, #967, .T. ) ;
#829 = CARTESIAN_POINT ( 'NONE',  ( 24.55500000000002103, 0.000000000000000000, 0.000000000000000000 ) ) ;
#831 = FACE_OUTER_BOUND ( 'NONE', #6393, .T. ) ;
#832 = VERTEX_POINT ( 'NONE', #214 ) ;
#833 = FACE_OUTER_BOUND ( 'NONE', #5763, .T. ) ;
#834 = CARTESIAN_POINT ( 'NONE',  ( 0.000000000000000000, 2.357898499370433054, -1.951563910473907981E-15 ) ) ;
#835 = AXIS2_PLACEMENT_3D ( 'NONE', #4055, #2668, #1934 ) ;
#836 = DIRECTION ( 'NONE',  ( -0.000000000000000000, 1.000000000000000000, -0.000000000000000000 ) ) ;
#837 = CARTESIAN_POINT ( 'NONE',  ( 347.0000000000000000, -4.999999999999998224, 145.0000000000000284 ) ) ;
#838 = ORIENTED_EDGE ( 'NONE', *, *, #2052, .F. ) ;
#839 = DIRECTION ( 'NONE',  ( -1.000000000000000000, 1.734723475976806848E-16, -0.000000000000000000 ) ) ;
#840 = VECTOR ( 'NONE', #844, 1000.000000000000000 ) ;
#841 = EDGE_CURVE ( 'NONE', #58, #2735, #4314, .T. ) ;
#842 = CARTESIAN_POINT ( 'NONE',  ( 0.000000000000000000, 0.000000000000000000, 140.0000000000000000 ) ) ;
#843 = DIRECTION ( 'NONE',  ( -0.000000000000000000, -0.000000000000000000, -1.000000000000000000 ) ) ;
#844 = DIRECTION ( 'NONE',  ( -1.000000000000000000, 1.734723475976806848E-16, -0.000000000000000000 ) ) ;
#845 = CYLINDRICAL_SURFACE ( 'NONE', #8071, 20.00000000000000000 ) ;
#846 = CARTESIAN_POINT ( 'NONE',  ( 5.200000000000002842, 3.061616997868384127E-16, -2.500000000000000888 ) ) ;
#847 = ORIENTED_EDGE ( 'NONE', *, *, #450, .T. ) ;
#848 = VERTEX_POINT ( 'NONE', #1578 ) ;
#849 = EDGE_CURVE ( 'NONE', #874, #3144, #1486, .T. ) ;
#850 = EDGE_CURVE ( 'NONE', #3060, #1959, #5615, .T. ) ;
#851 = EDGE_LOOP ( 'NONE', ( #4373, #2830 ) ) ;
#852 = PLANE ( 'NONE',  #6865 ) ;
#853 = ADVANCED_FACE ( 'NONE', ( #3012 ), #2366, .F. ) ;
#854 = DIRECTION ( 'NONE',  ( 1.000000000000000000, 0.000000000000000000, 0.000000000000000000 ) ) ;
#855 = ORIENTED_EDGE ( 'NONE', *, *, #4193, .F. ) ;
#856 = FACE_OUTER_BOUND ( 'NONE', #7874, .T. ) ;
#857 = ORIENTED_EDGE ( 'NONE', *, *, #6610, .T. ) ;
#858 = CARTESIAN_POINT ( 'NONE',  ( 5.000000000000000000, -5.000000000000000000, -0.9999999999999940048 ) ) ;
#859 = DIRECTION ( 'NONE',  ( -0.000000000000000000, 1.000000000000000000, -0.000000000000000000 ) ) ;
#860 = CONTEXT_DEPENDENT_SHAPE_REPRESENTATION ( #7649, #4681 ) ;
#861 = ORIENTED_EDGE ( 'NONE', *, *, #3272, .T. ) ;
#862 = ORIENTED_EDGE ( 'NONE', *, *, #1306, .F. ) ;
#863 = VERTEX_POINT ( 'NONE', #858 ) ;
#864 = DIRECTION ( 'NONE',  ( -1.000000000000000000, 0.000000000000000000, 0.000000000000000000 ) ) ;
#865 = AXIS2_PLACEMENT_3D ( 'NONE', #8225, #5756, #7156 ) ;
#866 = CARTESIAN_POINT ( 'NONE',  ( 2.548804901056335857E-15, 4.736522675502163437, -3.681124513963624612 ) ) ;
#867 = DIRECTION ( 'NONE',  ( 0.000000000000000000, 0.000000000000000000, -1.000000000000000000 ) ) ;
#868 = CARTESIAN_POINT ( 'NONE',  ( 10.00000000000000000, 0.000000000000000000, -97.99999999999997158 ) ) ;
#869 = CARTESIAN_POINT ( 'NONE',  ( 3.861362476283255685, 2.629030857715988656, -3.671615880910370500 ) ) ;
#870 = ORIENTED_EDGE ( 'NONE', *, *, #6832, .T. ) ;
#871 = AXIS2_PLACEMENT_3D ( 'NONE', #6654, #7187, #699 ) ;
#872 = SHAPE_REPRESENTATION ( 'single rail^MAS-188', ( #594 ), #4077 ) ;
#873 = DIRECTION ( 'NONE',  ( -0.000000000000000000, 1.000000000000000000, -0.000000000000000000 ) ) ;
#874 = VERTEX_POINT ( 'NONE', #6131 ) ;
#875 = ORIENTED_EDGE ( 'NONE', *, *, #2374, .F. ) ;
#876 = AXIS2_PLACEMENT_3D ( 'NONE', #2223, #1481, #4744 ) ;
#877 = FACE_OUTER_BOUND ( 'NONE', #3003, .T. ) ;
#878 = FACE_BOUND ( 'NONE', #2157, .T. ) ;
#879 = AXIS2_PLACEMENT_3D ( 'NONE', #1387, #8493, #2531 ) ;
#880 = EDGE_CURVE ( 'NONE', #8131, #2382, #653, .T. ) ;
#881 = CONICAL_SURFACE ( 'NONE', #165, 4.000000000000000000, 0.8911886515913786111 ) ;
#882 = DIRECTION ( 'NONE',  ( 0.000000000000000000, 0.000000000000000000, 1.000000000000000000 ) ) ;
#883 = LINE ( 'NONE', #8289, #1936 ) ;
#884 = VERTEX_POINT ( 'NONE', #166 ) ;
#885 = CARTESIAN_POINT ( 'NONE',  ( -1.747541505913277282, 3.837784562140256650, -3.503702292528906526 ) ) ;
#886 = CARTESIAN_POINT ( 'NONE',  ( -5.000000000000001776, 5.000000000000001776, 148.0000000000000284 ) ) ;
#887 =( GEOMETRIC_REPRESENTATION_CONTEXT ( 3 ) GLOBAL_UNCERTAINTY_ASSIGNED_CONTEXT ( ( #2680 ) ) GLOBAL_UNIT_ASSIGNED_CONTEXT ( ( #7558, #8174, #943 ) ) REPRESENTATION_CONTEXT ( 'NONE', 'WORKASPACE' ) );
#888 = CARTESIAN_POINT ( 'NONE',  ( -5.000000000000000000, -5.000000000000000000, 140.0000000000000000 ) ) ;
#889 = LINE ( 'NONE', #3543, #2783 ) ;
#890 = CARTESIAN_POINT ( 'NONE',  ( 0.000000000000000000, 0.000000000000000000, -43.99999999999997158 ) ) ;
#891 = DIRECTION ( 'NONE',  ( 0.000000000000000000, -1.000000000000000000, 1.287488025362403787E-15 ) ) ;
#892 = VECTOR ( 'NONE', #2203, 1000.000000000000000 ) ;
#893 = ORIENTED_EDGE ( 'NONE', *, *, #8129, .F. ) ;
#894 = ORIENTED_EDGE ( 'NONE', *, *, #3357, .F. ) ;
#895 = LINE ( 'NONE', #6196, #787 ) ;
#896 = DIRECTION ( 'NONE',  ( -0.000000000000000000, -0.000000000000000000, 1.000000000000000000 ) ) ;
#897 = LINE ( 'NONE', #3421, #3661 ) ;
#898 = VECTOR ( 'NONE', #7582, 1000.000000000000000 ) ;
#899 = EDGE_CURVE ( 'NONE', #884, #8142, #2838, .T. ) ;
#900 = ADVANCED_FACE ( 'NONE', ( #8155 ), #4838, .F. ) ;
#901 = ORIENTED_EDGE ( 'NONE', *, *, #7008, .T. ) ;
#902 = DIRECTION ( 'NONE',  ( 0.000000000000000000, -0.000000000000000000, -1.000000000000000000 ) ) ;
#903 = EDGE_LOOP ( 'NONE', ( #3099, #6280, #8023, #6203 ) ) ;
#904 = CARTESIAN_POINT ( 'NONE',  ( -31.74999999999995737, 3.061616997868384127E-16, -2.500000000000000888 ) ) ;
#905 = DIRECTION ( 'NONE',  ( 0.000000000000000000, 0.000000000000000000, -1.000000000000000000 ) ) ;
#906 = PRODUCT_CONTEXT ( 'NONE', #5527, 'mechanical' ) ;
#907 = DIRECTION ( 'NONE',  ( 0.000000000000000000, 0.000000000000000000, -1.000000000000000000 ) ) ;
#908 = ORIENTED_EDGE ( 'NONE', *, *, #5601, .F. ) ;
#909 = ORIENTED_EDGE ( 'NONE', *, *, #279, .T. ) ;
#910 = CARTESIAN_POINT ( 'NONE',  ( 0.2500000000000002220, 0.000000000000000000, 0.000000000000000000 ) ) ;
#911 = FACE_OUTER_BOUND ( 'NONE', #8041, .T. ) ;
#912 = DIRECTION ( 'NONE',  ( -0.000000000000000000, 1.000000000000000000, -0.000000000000000000 ) ) ;
#913 = CARTESIAN_POINT ( 'NONE',  ( 4.175648173966055587, -2.207990556236547608, -3.469390959564065291 ) ) ;
#914 = EDGE_CURVE ( 'NONE', #6725, #5979, #5528, .T. ) ;
#915 = EDGE_LOOP ( 'NONE', ( #5258, #2722, #7340, #8456, #7652 ) ) ;
#916 = DIRECTION ( 'NONE',  ( -1.000000000000000000, 0.000000000000000000, 0.000000000000000000 ) ) ;
#917 = VERTEX_POINT ( 'NONE', #3142 ) ;
#918 = ORIENTED_EDGE ( 'NONE', *, *, #4465, .T. ) ;
#919 = AXIS2_PLACEMENT_3D ( 'NONE', #4469, #2522, #7750 ) ;
#920 = CARTESIAN_POINT ( 'NONE',  ( 347.0000000000000000, -4.999999999999998224, 139.9990000000000236 ) ) ;
#921 = FACE_BOUND ( 'NONE', #2013, .T. ) ;
#922 =( REPRESENTATION_RELATIONSHIP ('NONE','NONE', #3312, #1479 ) REPRESENTATION_RELATIONSHIP_WITH_TRANSFORMATION ( #6946 )SHAPE_REPRESENTATION_RELATIONSHIP( ) );
#923 = CARTESIAN_POINT ( 'NONE',  ( 5.000000000000002665, 0.000000000000000000, -2.700000000000001066 ) ) ;
#924 = VECTOR ( 'NONE', #6380, 1000.000000000000000 ) ;
#925 = FACE_BOUND ( 'NONE', #8290, .T. ) ;
#926 = VERTEX_POINT ( 'NONE', #5784 ) ;
#927 = DIRECTION ( 'NONE',  ( -0.000000000000000000, 0.000000000000000000, -1.000000000000000000 ) ) ;
#928 = CARTESIAN_POINT ( 'NONE',  ( 470.0000000000000000, 15.00000000000000000, 140.0000000000000000 ) ) ;
#929 = AXIS2_PLACEMENT_3D ( 'NONE', #4850, #7548, #4148 ) ;
#930 = CIRCLE ( 'NONE', #5649, 10.00000000000000000 ) ;
#931 = DIRECTION ( 'NONE',  ( 0.000000000000000000, 0.000000000000000000, 1.000000000000000000 ) ) ;
#932 = ADVANCED_FACE ( 'NONE', ( #8459, #2497 ), #5699, .T. ) ;
#933 = DIRECTION ( 'NONE',  ( 0.000000000000000000, 0.000000000000000000, 1.000000000000000000 ) ) ;
#934 = EDGE_CURVE ( 'NONE', #1995, #7568, #485, .T. ) ;
#935 = VECTOR ( 'NONE', #357, 1000.000000000000000 ) ;
#936 = CARTESIAN_POINT ( 'NONE',  ( -5.000000000000000000, -5.000000000000000000, 42.00000000000000711 ) ) ;
#937 = AXIS2_PLACEMENT_3D ( 'NONE', #5438, #5912, #7446 ) ;
#938 = ORIENTED_EDGE ( 'NONE', *, *, #3732, .F. ) ;
#939 = EDGE_CURVE ( 'NONE', #3102, #1905, #6485, .T. ) ;
#940 = ORIENTED_EDGE ( 'NONE', *, *, #2023, .F. ) ;
#941 = ORIENTED_EDGE ( 'NONE', *, *, #8359, .F. ) ;
#942 = DIRECTION ( 'NONE',  ( 0.000000000000000000, 0.000000000000000000, -1.000000000000000000 ) ) ;
#943 =( NAMED_UNIT ( * ) SI_UNIT ( $, .STERADIAN. ) SOLID_ANGLE_UNIT ( ) );
#944 = ORIENTED_EDGE ( 'NONE', *, *, #7928, .F. ) ;
#945 = LINE ( 'NONE', #6810, #2868 ) ;
#946 = COLOUR_RGB ( '',0.8941176470588234615, 0.8941176470588234615, 0.8941176470588234615 ) ;
#947 = ORIENTED_EDGE ( 'NONE', *, *, #3635, .F. ) ;
#948 = ADVANCED_FACE ( 'NONE', ( #4443 ), #561, .F. ) ;
#949 = DIRECTION ( 'NONE',  ( 0.000000000000000000, 0.000000000000000000, 1.000000000000000000 ) ) ;
#950 = FACE_OUTER_BOUND ( 'NONE', #3769, .T. ) ;
#951 = VERTEX_POINT ( 'NONE', #3223 ) ;
#952 = EDGE_LOOP ( 'NONE', ( #6894, #7607 ) ) ;
#953 = EDGE_CURVE ( 'NONE', #7048, #8019, #4248, .T. ) ;
#954 = LINE ( 'NONE', #6033, #1288 ) ;
#955 = LINE ( 'NONE', #3606, #3821 ) ;
#956 = CARTESIAN_POINT ( 'NONE',  ( -2.804994570502171047, -3.229033611042465335, -3.526374918436838701 ) ) ;
#957 = CARTESIAN_POINT ( 'NONE',  ( 219.9999999999999716, -20.00000000000000000, 162.5000000000000853 ) ) ;
#958 = VERTEX_POINT ( 'NONE', #1835 ) ;
#959 = VECTOR ( 'NONE', #4708, 1000.000000000000000 ) ;
#960 = DIRECTION ( 'NONE',  ( 1.000000000000000000, 0.000000000000000000, 0.000000000000000000 ) ) ;
#961 = CARTESIAN_POINT ( 'NONE',  ( 0.000000000000000000, -1.178949249685213863, 2.042000000000002924 ) ) ;
#962 = ORIENTED_EDGE ( 'NONE', *, *, #7523, .T. ) ;
#963 = ORIENTED_EDGE ( 'NONE', *, *, #338, .T. ) ;
#964 = DIRECTION ( 'NONE',  ( -0.8660254037844373753, 0.5000000000000021094, 0.000000000000000000 ) ) ;
#965 = CARTESIAN_POINT ( 'NONE',  ( -30.00000000000002842, -20.00000000000000000, 200.0000000000000000 ) ) ;
#966 = AXIS2_PLACEMENT_3D ( 'NONE', #6013, #2106, #2634 ) ;
#967 = LINE ( 'NONE', #3617, #795 ) ;
#968 = LINE ( 'NONE', #7447, #1506 ) ;
#969 = ORIENTED_EDGE ( 'NONE', *, *, #7360, .F. ) ;
#970 = PLANE ( 'NONE',  #4855 ) ;
#971 = AXIS2_PLACEMENT_3D ( 'NONE', #2426, #571, #8551 ) ;
#972 = CARTESIAN_POINT ( 'NONE',  ( -30.00000000000002842, -20.00000000000000000, 180.0000000000000284 ) ) ;
#973 = CARTESIAN_POINT ( 'NONE',  ( -10.00000000000000000, 1.224646799147353256E-15, -43.99999999999997158 ) ) ;
#974 = AXIS2_PLACEMENT_3D ( 'NONE', #6798, #8163, #2152 ) ;
#975 = PLANE ( 'NONE',  #4861 ) ;
#976 = EDGE_CURVE ( 'NONE', #3444, #530, #354, .T. ) ;
#977 = FACE_OUTER_BOUND ( 'NONE', #5652, .T. ) ;
#978 = DIRECTION ( 'NONE',  ( 0.000000000000000000, 1.000000000000000000, 0.000000000000000000 ) ) ;
#979 = ORIENTED_EDGE ( 'NONE', *, *, #3323, .F. ) ;
#980 = ORIENTED_EDGE ( 'NONE', *, *, #7467, .T. ) ;
#981 = EDGE_CURVE ( 'NONE', #7356, #8085, #7140, .T. ) ;
#982 = ORIENTED_EDGE ( 'NONE', *, *, #4280, .T. ) ;
#983 = CARTESIAN_POINT ( 'NONE',  ( -10.00000000000000000, 1.224646799147353256E-15, 42.00000000000000711 ) ) ;
#984 = ADVANCED_FACE ( 'NONE', ( #1052 ), #524, .F. ) ;
#985 = DIRECTION ( 'NONE',  ( -0.000000000000000000, 0.000000000000000000, -1.000000000000000000 ) ) ;
#986 = ADVANCED_FACE ( 'NONE', ( #8495 ), #7673, .F. ) ;
#987 = ORIENTED_EDGE ( 'NONE', *, *, #3596, .T. ) ;
#988 = CARTESIAN_POINT ( 'NONE',  ( 0.000000000000000000, 0.000000000000000000, -25.03750572909317285 ) ) ;
#989 = VERTEX_POINT ( 'NONE', #3745 ) ;
#990 = CARTESIAN_POINT ( 'NONE',  ( -20.00000000000000000, 2.449293598294706513E-15, -84.56854249492380404 ) ) ;
#991 = ORIENTED_EDGE ( 'NONE', *, *, #2182, .F. ) ;
#992 = ORIENTED_EDGE ( 'NONE', *, *, #2383, .F. ) ;
#993 = DIRECTION ( 'NONE',  ( -1.000000000000000000, 0.000000000000000000, 0.000000000000000000 ) ) ;
#994 = CARTESIAN_POINT ( 'NONE',  ( -5.000000000000000000, -5.000000000000000000, 140.0000000000000000 ) ) ;
#995 = CARTESIAN_POINT ( 'NONE',  ( 88.00000000000000000, -20.00000000000000000, -121.8314250403154659 ) ) ;
#996 = DIRECTION ( 'NONE',  ( 0.000000000000000000, 1.000000000000000000, 0.000000000000000000 ) ) ;
#997 = VERTEX_POINT ( 'NONE', #1752 ) ;
#998 = DIRECTION ( 'NONE',  ( 1.000000000000000000, 0.000000000000000000, 0.000000000000000000 ) ) ;
#999 = DIRECTION ( 'NONE',  ( -0.000000000000000000, -0.000000000000000000, 1.000000000000000000 ) ) ;
#1000 = ORIENTED_EDGE ( 'NONE', *, *, #1573, .F. ) ;
#1001 = ORIENTED_EDGE ( 'NONE', *, *, #282, .F. ) ;
#1002 = CARTESIAN_POINT ( 'NONE',  ( -5.000000000000000000, -5.000000000000000000, 140.0000000000000000 ) ) ;
#1003 = LINE ( 'NONE', #3657, #761 ) ;
#1004 = CARTESIAN_POINT ( 'NONE',  ( 0.000000000000000000, -25.00000000000000000, -154.8500000000000512 ) ) ;
#1005 = VECTOR ( 'NONE', #2734, 1000.000000000000000 ) ;
#1006 = CARTESIAN_POINT ( 'NONE',  ( 264.0000000000000000, -20.00000000000000000, -54.08142504031544462 ) ) ;
#1007 = EDGE_CURVE ( 'NONE', #1337, #765, #4805, .T. ) ;
#1008 = FACE_BOUND ( 'NONE', #1463, .T. ) ;
#1009 = VERTEX_POINT ( 'NONE', #3878 ) ;
#1010 = ADVANCED_FACE ( 'NONE', ( #6523 ), #8539, .F. ) ;
#1011 = CARTESIAN_POINT ( 'NONE',  ( 0.000000000000000000, 0.000000000000000000, 42.00000000000000711 ) ) ;
#1012 = TOROIDAL_SURFACE ( 'NONE', #7821, 5.384454397937118664, 0.5155456020628804703 ) ;
#1013 = VERTEX_POINT ( 'NONE', #1709 ) ;
#1014 = CARTESIAN_POINT ( 'NONE',  ( -4.999999999999998224, 5.000000000000001776, 139.9990000000000236 ) ) ;
#1015 = DIRECTION ( 'NONE',  ( 1.000000000000000000, 0.000000000000000000, -0.000000000000000000 ) ) ;
#1016 = VECTOR ( 'NONE', #239, 1000.000000000000000 ) ;
#1017 = ADVANCED_FACE ( 'NONE', ( #7760 ), #5634, .T. ) ;
#1018 = DIRECTION ( 'NONE',  ( -0.000000000000000000, -0.000000000000000000, 1.000000000000000000 ) ) ;
#1019 = VECTOR ( 'NONE', #8238, 1000.000000000000000 ) ;
#1020 = DIRECTION ( 'NONE',  ( -0.000000000000000000, -0.000000000000000000, 1.000000000000000000 ) ) ;
#1021 = CARTESIAN_POINT ( 'NONE',  ( -4.000000000000000000, 1.677772373332757194, -3.535253723897187506 ) ) ;
#1023 = ORIENTED_EDGE ( 'NONE', *, *, #5149, .T. ) ;
#1022 = PRODUCT_RELATED_PRODUCT_CATEGORY ( 'part', '', ( #654 ) ) ;
#1024 = VECTOR ( 'NONE', #8001, 1000.000000000000000 ) ;
#1025 = PRESENTATION_LAYER_ASSIGNMENT (  '', '', ( #5185 ) ) ;
#1026 = VERTEX_POINT ( 'NONE', #7719 ) ;
#1027 = ORIENTED_EDGE ( 'NONE', *, *, #1401, .F. ) ;
#1028 = DIRECTION ( 'NONE',  ( -1.000000000000000000, 0.000000000000000000, -0.000000000000000000 ) ) ;
#1029 = PLANE ( 'NONE',  #4496 ) ;
#1030 = CIRCLE ( 'NONE', #7985, 10.00000000000000000 ) ;
#1031 = EDGE_LOOP ( 'NONE', ( #8342, #5767, #3173, #2916 ) ) ;
#1032 = DIRECTION ( 'NONE',  ( -1.734723475976806848E-16, -1.000000000000000000, 0.000000000000000000 ) ) ;
#1033 = VERTEX_POINT ( 'NONE', #4401 ) ;
#1034 = CARTESIAN_POINT ( 'NONE',  ( -5.000000000000001776, 5.000000000000001776, 140.0000000000000000 ) ) ;
#1035 = CONTEXT_DEPENDENT_SHAPE_REPRESENTATION ( #3196, #1083 ) ;
#1036 = ORIENTED_EDGE ( 'NONE', *, *, #1548, .T. ) ;
#1037 = ORIENTED_EDGE ( 'NONE', *, *, #3856, .T. ) ;
#1038 = AXIS2_PLACEMENT_3D ( 'NONE', #8058, #6557, #6521 ) ;
#1039 = CARTESIAN_POINT ( 'NONE',  ( -4.197393957002303999, -7.773935952363655451E-14, -3.503767560748929810 ) ) ;
#1040 = CARTESIAN_POINT ( 'NONE',  ( -5.000000000000000000, -5.000000000000000000, 148.0000000000000284 ) ) ;
#1041 = LINE ( 'NONE', #335, #4655 ) ;
#1042 = CARTESIAN_POINT ( 'NONE',  ( 386.6666666666666288, -15.00000000000000000, 162.5000000000000853 ) ) ;
#1043 = EDGE_CURVE ( 'NONE', #3807, #1428, #7052, .T. ) ;
#1044 = VERTEX_POINT ( 'NONE', #3097 ) ;
#1045 = DIRECTION ( 'NONE',  ( 6.123233995736766036E-17, -1.000000000000000000, 0.000000000000000000 ) ) ;
#1046 = DIRECTION ( 'NONE',  ( 0.000000000000000000, 1.000000000000000000, 0.000000000000000000 ) ) ;
#1047 = ORIENTED_EDGE ( 'NONE', *, *, #1141, .T. ) ;
#1048 = ADVANCED_FACE ( 'NONE', ( #8418 ), #2454, .F. ) ;
#1049 = EDGE_LOOP ( 'NONE', ( #7724, #3053, #1355, #2617 ) ) ;
#1050 = DIRECTION ( 'NONE',  ( 0.000000000000000000, 0.000000000000000000, 1.000000000000000000 ) ) ;
#1051 = DIRECTION ( 'NONE',  ( 0.000000000000000000, 0.000000000000000000, 1.000000000000000000 ) ) ;
#1052 = FACE_OUTER_BOUND ( 'NONE', #5062, .T. ) ;
#1053 = PLANE ( 'NONE',  #7902 ) ;
#1054 = ORIENTED_EDGE ( 'NONE', *, *, #7248, .T. ) ;
#1055 = DIRECTION ( 'NONE',  ( -1.000000000000000000, 0.000000000000000000, 0.000000000000000000 ) ) ;
#1056 = ORIENTED_EDGE ( 'NONE', *, *, #1919, .T. ) ;
#1057 = CARTESIAN_POINT ( 'NONE',  ( 4.211140560182196957, 2.431303136016536470, -3.745885042887433514 ) ) ;
#1058 = ADVANCED_FACE ( 'NONE', ( #8581 ), #3438, .F. ) ;
#1059 = AXIS2_PLACEMENT_3D ( 'NONE', #7436, #2132, #1562 ) ;
#1060 = CARTESIAN_POINT ( 'NONE',  ( 470.0000000000000000, -20.00000000000000000, 200.0000000000000000 ) ) ;
#1061 = DIRECTION ( 'NONE',  ( 1.000000000000000000, 0.000000000000000000, 0.000000000000000000 ) ) ;
#1062 = FILL_AREA_STYLE_COLOUR ( '', #3712 ) ;
#1063 = ORIENTED_EDGE ( 'NONE', *, *, #1301, .F. ) ;
#1064 = VECTOR ( 'NONE', #2605, 1000.000000000000000 ) ;
#1065 = AXIS2_PLACEMENT_3D ( 'NONE', #2120, #1381, #4039 ) ;
#1066 = ORIENTED_EDGE ( 'NONE', *, *, #5474, .F. ) ;
#1067 = LINE ( 'NONE', #8387, #5879 ) ;
#1068 = FACE_OUTER_BOUND ( 'NONE', #2118, .T. ) ;
#1069 = UNCERTAINTY_MEASURE_WITH_UNIT (LENGTH_MEASURE( 1.000000000000000082E-05 ), #4318, 'distance_accuracy_value', 'NONE');
#1070 = AXIS2_PLACEMENT_3D ( 'NONE', #7504, #6235, #269 ) ;
#1071 = AXIS2_PLACEMENT_3D ( 'NONE', #1162, #2440, #3166 ) ;
#1072 = ORIENTED_EDGE ( 'NONE', *, *, #5520, .F. ) ;
#1073 = FACE_OUTER_BOUND ( 'NONE', #5412, .T. ) ;
#1074 = ORIENTED_EDGE ( 'NONE', *, *, #175, .T. ) ;
#1075 = FACE_BOUND ( 'NONE', #2339, .T. ) ;
#1076 = CONTEXT_DEPENDENT_SHAPE_REPRESENTATION ( #5688, #1563 ) ;
#1077 = VERTEX_POINT ( 'NONE', #6603 ) ;
#1078 = ORIENTED_EDGE ( 'NONE', *, *, #5149, .F. ) ;
#1079 = DIRECTION ( 'NONE',  ( -0.000000000000000000, 0.000000000000000000, 1.000000000000000000 ) ) ;
#1080 = CARTESIAN_POINT ( 'NONE',  ( 5.000000000000000000, -5.000000000000000000, 140.0000000000000000 ) ) ;
#1081 = APPLICATION_CONTEXT ( 'automotive_design' ) ;
#1082 = CARTESIAN_POINT ( 'NONE',  ( 4.198928548860774157, -0.8158838809860124996, -3.526471437616918170 ) ) ;
#1083 = PRODUCT_DEFINITION_SHAPE ( 'NONE', 'NONE',  #8621 ) ;
#1084 = CARTESIAN_POINT ( 'NONE',  ( 347.0000000000000000, 5.000000000000001776, 145.0000000000000284 ) ) ;
#1085 = ORIENTED_EDGE ( 'NONE', *, *, #1626, .F. ) ;
#1086 = DIRECTION ( 'NONE',  ( 1.000000000000000000, 6.123233995736766036E-17, -6.123233995736764803E-17 ) ) ;
#1087 = DIRECTION ( 'NONE',  ( 0.000000000000000000, 0.000000000000000000, -1.000000000000000000 ) ) ;
#1088 = ORIENTED_EDGE ( 'NONE', *, *, #2206, .F. ) ;
#1089 = VERTEX_POINT ( 'NONE', #8017 ) ;
#1090 = EDGE_CURVE ( 'NONE', #5384, #1324, #2588, .T. ) ;
#1091 = CARTESIAN_POINT ( 'NONE',  ( 0.000000000000000000, 0.000000000000000000, 140.0000000000000000 ) ) ;
#1092 = CARTESIAN_POINT ( 'NONE',  ( -4.999999999999998224, 5.000000000000001776, 145.0000000000000284 ) ) ;
#1093 = EDGE_CURVE ( 'NONE', #1691, #6087, #7352, .T. ) ;
#1094 = EDGE_CURVE ( 'NONE', #5639, #3374, #29, .T. ) ;
#1095 = CARTESIAN_POINT ( 'NONE',  ( -5.000000000000000000, -5.000000000000000000, -143.0000000000000284 ) ) ;
#1096 = AXIS2_PLACEMENT_3D ( 'NONE', #304, #5616, #6747 ) ;
#1097 = DIRECTION ( 'NONE',  ( -1.000000000000000000, 0.000000000000000000, -0.000000000000000000 ) ) ;
#1098 = ORIENTED_EDGE ( 'NONE', *, *, #8359, .T. ) ;
#1099 = SURFACE_STYLE_FILL_AREA ( #3840 ) ;
#1100 = ORIENTED_EDGE ( 'NONE', *, *, #2407, .F. ) ;
#1101 = CARTESIAN_POINT ( 'NONE',  ( 1.390230914382191596, 4.043987460488659202, -3.502507215260488582 ) ) ;
#1102 = CIRCLE ( 'NONE', #966, 10.00000000000000000 ) ;
#1103 = CARTESIAN_POINT ( 'NONE',  ( 0.000000000000000000, 0.000000000000000000, 120.0000000000000142 ) ) ;
#1104 = DIRECTION ( 'NONE',  ( -0.000000000000000000, -0.000000000000000000, -1.000000000000000000 ) ) ;
#1105 = LINE ( 'NONE', #1146, #3062 ) ;
#1106 = CARTESIAN_POINT ( 'NONE',  ( -4.000000000000000000, 0.8576368993457507139, -3.433240632782198709 ) ) ;
#1107 = VECTOR ( 'NONE', #7729, 1000.000000000000000 ) ;
#1108 = ORIENTED_EDGE ( 'NONE', *, *, #5934, .F. ) ;
#1109 = FILL_AREA_STYLE ('',( #451 ) ) ;
#1110 = CARTESIAN_POINT ( 'NONE',  ( -20.00000000000000000, 140.0000000000000000, 5.000000000000000000 ) ) ;
#1111 = DIRECTION ( 'NONE',  ( -1.000000000000000000, 0.000000000000000000, -0.000000000000000000 ) ) ;
#1112 = DIRECTION ( 'NONE',  ( 0.000000000000000000, 0.000000000000000000, 1.000000000000000000 ) ) ;
#1113 = CIRCLE ( 'NONE', #5961, 10.00000000000000000 ) ;
#1114 = VERTEX_POINT ( 'NONE', #784 ) ;
#1115 = LINE ( 'NONE', #6375, #6752 ) ;
#1116 = ADVANCED_FACE ( 'NONE', ( #1925 ), #7880, .F. ) ;
#1117 = VERTEX_POINT ( 'NONE', #3352 ) ;
#1118 = EDGE_CURVE ( 'NONE', #1114, #771, #5655, .T. ) ;
#1119 = DIRECTION ( 'NONE',  ( 0.000000000000000000, 0.000000000000000000, 1.000000000000000000 ) ) ;
#1120 = AXIS2_PLACEMENT_3D ( 'NONE', #2318, #4961, #4307 ) ;
#1121 = ORIENTED_EDGE ( 'NONE', *, *, #2127, .F. ) ;
#1122 = ADVANCED_FACE ( 'NONE', ( #737 ), #4478, .F. ) ;
#1123 = VERTEX_POINT ( 'NONE', #2089 ) ;
#1124 = CARTESIAN_POINT ( 'NONE',  ( 219.9999999999999716, -20.00000000000000000, 159.8500000000001080 ) ) ;
#1125 = DIRECTION ( 'NONE',  ( 1.000000000000000000, 0.000000000000000000, 0.000000000000000000 ) ) ;
#1126 = FACE_OUTER_BOUND ( 'NONE', #2316, .T. ) ;
#1127 = ORIENTED_EDGE ( 'NONE', *, *, #3594, .F. ) ;
#1128 = CARTESIAN_POINT ( 'NONE',  ( 136.6666666666666288, -10.00000000000000000, 162.5000000000000853 ) ) ;
#1129 = ADVANCED_FACE ( 'NONE', ( #609 ), #3265, .F. ) ;
#1130 = DIRECTION ( 'NONE',  ( 1.000000000000000000, 0.000000000000000000, 0.000000000000000000 ) ) ;
#1131 = ORIENTED_EDGE ( 'NONE', *, *, #6482, .F. ) ;
#1132 = ORIENTED_EDGE ( 'NONE', *, *, #1493, .F. ) ;
#1133 = CARTESIAN_POINT ( 'NONE',  ( 5.000000000000000000, 5.000000000000000000, -135.0000000000000000 ) ) ;
#1134 = LINE ( 'NONE', #5133, #3405 ) ;
#1135 = DIRECTION ( 'NONE',  ( -1.000000000000000000, 0.000000000000000000, 0.000000000000000000 ) ) ;
#1136 = MECHANICAL_DESIGN_GEOMETRIC_PRESENTATION_REPRESENTATION (  '', ( #3632 ), #5713 ) ;
#1137 = DIRECTION ( 'NONE',  ( 0.000000000000000000, -0.000000000000000000, 1.000000000000000000 ) ) ;
#1138 = ORIENTED_EDGE ( 'NONE', *, *, #4139, .F. ) ;
#1139 = ORIENTED_EDGE ( 'NONE', *, *, #4828, .F. ) ;
#1140 = DIRECTION ( 'NONE',  ( 0.000000000000000000, 0.000000000000000000, 1.000000000000000000 ) ) ;
#1141 = EDGE_CURVE ( 'NONE', #6628, #563, #8296, .T. ) ;
#1142 = AXIS2_PLACEMENT_3D ( 'NONE', #8007, #3909, #8573 ) ;
#1143 = CIRCLE ( 'NONE', #1708, 10.00000000000000000 ) ;
#1144 = DIRECTION ( 'NONE',  ( -0.000000000000000000, -0.000000000000000000, 1.000000000000000000 ) ) ;
#1145 = CARTESIAN_POINT ( 'NONE',  ( 269.0000000000000000, -4.999999999999998224, 145.0000000000000284 ) ) ;
#1146 = CARTESIAN_POINT ( 'NONE',  ( 2.500000000000000000, -1.178949249685213863, 2.042000000000002924 ) ) ;
#1147 = DIRECTION ( 'NONE',  ( 1.000000000000000000, 0.000000000000000000, 0.000000000000000000 ) ) ;
#1148 = ADVANCED_FACE ( 'NONE', ( #4120, #814 ), #4158, .T. ) ;
#1149 = EDGE_CURVE ( 'NONE', #3461, #2983, #5389, .T. ) ;
#1150 = ORIENTED_EDGE ( 'NONE', *, *, #4489, .F. ) ;
#1151 = VECTOR ( 'NONE', #7357, 1000.000000000000000 ) ;
#1152 = ADVANCED_FACE ( 'NONE', ( #3482 ), #8277, .T. ) ;
#1153 = VECTOR ( 'NONE', #1857, 1000.000000000000000 ) ;
#1154 = FACE_OUTER_BOUND ( 'NONE', #3518, .T. ) ;
#1155 = DIRECTION ( 'NONE',  ( -1.000000000000000000, 0.000000000000000000, 0.000000000000000000 ) ) ;
#1156 = VECTOR ( 'NONE', #4836, 999.9999999999998863 ) ;
#1157 = VECTOR ( 'NONE', #4825, 999.9999999999998863 ) ;
#1158 = DIRECTION ( 'NONE',  ( 0.000000000000000000, -1.000000000000000000, 0.000000000000000000 ) ) ;
#1159 = CIRCLE ( 'NONE', #4764, 2.649999999999993694 ) ;
#1160 = VERTEX_POINT ( 'NONE', #4912 ) ;
#1161 =( LENGTH_UNIT ( ) NAMED_UNIT ( * ) SI_UNIT ( .MILLI., .METRE. ) );
#1162 = CARTESIAN_POINT ( 'NONE',  ( 0.000000000000000000, 0.000000000000000000, -97.99999999999997158 ) ) ;
#1163 = ORIENTED_EDGE ( 'NONE', *, *, #4970, .T. ) ;
#1164 = DIRECTION ( 'NONE',  ( -1.000000000000000000, 0.000000000000000000, 0.000000000000000000 ) ) ;
#1165 = VECTOR ( 'NONE', #4331, 1000.000000000000000 ) ;
#1166 = LINE ( 'NONE', #5806, #2003 ) ;
#1167 =( GEOMETRIC_REPRESENTATION_CONTEXT ( 3 ) GLOBAL_UNCERTAINTY_ASSIGNED_CONTEXT ( ( #7375 ) ) GLOBAL_UNIT_ASSIGNED_CONTEXT ( ( #5199, #5155, #8515 ) ) REPRESENTATION_CONTEXT ( 'NONE', 'WORKASPACE' ) );
#1168 = EDGE_CURVE ( 'NONE', #8068, #1823, #2321, .T. ) ;
#1169 = ADVANCED_FACE ( 'NONE', ( #2314 ), #6779, .F. ) ;
#1170 = DIRECTION ( 'NONE',  ( -1.000000000000000000, -0.000000000000000000, -0.000000000000000000 ) ) ;
#1171 = ORIENTED_EDGE ( 'NONE', *, *, #5798, .F. ) ;
#1172 = VECTOR ( 'NONE', #3157, 1000.000000000000000 ) ;
#1173 = DIRECTION ( 'NONE',  ( -2.324323025717218695E-17, 1.000000000000000000, -2.622289662148106525E-18 ) ) ;
#1174 = CARTESIAN_POINT ( 'NONE',  ( 219.9999999999999716, -20.00000000000000000, 162.5000000000000853 ) ) ;
#1175 = ORIENTED_EDGE ( 'NONE', *, *, #7440, .F. ) ;
#1176 = ADVANCED_BREP_SHAPE_REPRESENTATION ( '', ( #1852, #594 ), #5323 ) ;
#1177 = ORIENTED_EDGE ( 'NONE', *, *, #4810, .T. ) ;
#1178 = CARTESIAN_POINT ( 'NONE',  ( 219.9999999999999716, -20.00000000000000000, 165.1500000000000625 ) ) ;
#1179 = CARTESIAN_POINT ( 'NONE',  ( -6.259644161404860030E-16, -4.618802153517027165, -3.433295621305388234 ) ) ;
#1180 = AXIS2_PLACEMENT_3D ( 'NONE', #7920, #7259, #5945 ) ;
#1181 = ADVANCED_FACE ( 'NONE', ( #6300, #2784 ), #6256, .F. ) ;
#1182 = DIRECTION ( 'NONE',  ( -0.000000000000000000, -0.000000000000000000, -1.000000000000000000 ) ) ;
#1183 = CARTESIAN_POINT ( 'NONE',  ( 0.000000000000000000, 0.000000000000000000, 140.0000000000000000 ) ) ;
#1184 = ORIENTED_EDGE ( 'NONE', *, *, #3190, .F. ) ;
#1185 = ORIENTED_EDGE ( 'NONE', *, *, #201, .F. ) ;
#1186 = EDGE_LOOP ( 'NONE', ( #3554, #4363 ) ) ;
#1187 = CARTESIAN_POINT ( 'NONE',  ( 3.472371940585993855, 2.614027278893175321, -3.320322319201766792 ) ) ;
#1188 = B_SPLINE_CURVE_WITH_KNOTS ( 'NONE', 3,
 ( #3899, #6542, #5890, #5144, #1804, #8424 ),
 .UNSPECIFIED., .F., .F.,
 ( 4, 2, 4 ),
 ( 0.002365888236227977302, 0.003551327329835078910, 0.004736766423442180518 ),
 .UNSPECIFIED. ) ;
#1189 = FACE_BOUND ( 'NONE', #5501, .T. ) ;
#1190 = DIRECTION ( 'NONE',  ( 0.000000000000000000, 0.000000000000000000, 1.000000000000000000 ) ) ;
#1191 = AXIS2_PLACEMENT_3D ( 'NONE', #5725, #6385, #8316 ) ;
#1192 = DIRECTION ( 'NONE',  ( 0.000000000000000000, 1.000000000000000000, 0.000000000000000000 ) ) ;
#1193 = CARTESIAN_POINT ( 'NONE',  ( 2.500000000000000000, -1.768423874527823569, 1.021000000000002794 ) ) ;
#1194 = CARTESIAN_POINT ( 'NONE',  ( -5.000000000000001776, 5.000000000000001776, 148.0000000000000284 ) ) ;
#1195 = AXIS2_PLACEMENT_3D ( 'NONE', #7262, #694, #2743 ) ;
#1196 = CARTESIAN_POINT ( 'NONE',  ( -10.00000000000000000, 1.224646799147353256E-15, -135.0000000000000000 ) ) ;
#1197 = EDGE_CURVE ( 'NONE', #4852, #5678, #6117, .T. ) ;
#1198 = FACE_OUTER_BOUND ( 'NONE', #296, .T. ) ;
#1199 = EDGE_CURVE ( 'NONE', #2303, #806, #497, .T. ) ;
#1200 = ADVANCED_FACE ( 'NONE', ( #290 ), #2827, .F. ) ;
#1201 = VECTOR ( 'NONE', #7955, 1000.000000000000000 ) ;
#1202 = CYLINDRICAL_SURFACE ( 'NONE', #4532, 2.649999999999985700 ) ;
#1203 = AXIS2_PLACEMENT_3D ( 'NONE', #5420, #8139, #5288 ) ;
#1204 = ORIENTED_EDGE ( 'NONE', *, *, #4975, .T. ) ;
#1205 = CARTESIAN_POINT ( 'NONE',  ( 5.000000000000000000, 5.000000000000000000, 34.00000000000000711 ) ) ;
#1206 = ORIENTED_EDGE ( 'NONE', *, *, #7099, .F. ) ;
#1207 = LINE ( 'NONE', #3864, #3823 ) ;
#1208 = FACE_OUTER_BOUND ( 'NONE', #8313, .T. ) ;
#1209 = CIRCLE ( 'NONE', #8452, 0.2500000000000002220 ) ;
#1210 = CARTESIAN_POINT ( 'NONE',  ( 434.9999999999999432, -4.999999999999998224, 139.9990000000000236 ) ) ;
#1211 = ORIENTED_EDGE ( 'NONE', *, *, #3119, .F. ) ;
#1212 = DIRECTION ( 'NONE',  ( -1.000000000000000000, 1.734723475976807341E-16, -0.000000000000000000 ) ) ;
#1213 = EDGE_CURVE ( 'NONE', #730, #716, #6215, .T. ) ;
#1214 = PRODUCT_CONTEXT ( 'NONE', #5844, 'mechanical' ) ;
#1215 = CARTESIAN_POINT ( 'NONE',  ( 0.2500000000000002220, 0.000000000000000000, 0.000000000000000000 ) ) ;
#1216 = EDGE_LOOP ( 'NONE', ( #2370, #6915, #754, #504 ) ) ;
#1217 = ORIENTED_EDGE ( 'NONE', *, *, #8059, .F. ) ;
#1218 = CARTESIAN_POINT ( 'NONE',  ( -5.000000000000001776, 5.000000000000001776, 140.0000000000000000 ) ) ;
#1219 = CARTESIAN_POINT ( 'NONE',  ( 88.00000000000000000, -25.00000000000000000, -119.1814250403154745 ) ) ;
#1220 = DIRECTION ( 'NONE',  ( -1.000000000000000000, -0.000000000000000000, -0.000000000000000000 ) ) ;
#1221 = DIRECTION ( 'NONE',  ( 1.000000000000000000, 0.000000000000000000, 0.000000000000000000 ) ) ;
#1222 = ORIENTED_EDGE ( 'NONE', *, *, #2485, .T. ) ;
#1223 = VECTOR ( 'NONE', #3407, 1000.000000000000000 ) ;
#1224 = ORIENTED_EDGE ( 'NONE', *, *, #7346, .T. ) ;
#1225 = CARTESIAN_POINT ( 'NONE',  ( 5.000000000000000000, 5.000000000000000000, -135.0000000000000000 ) ) ;
#1226 = EDGE_CURVE ( 'NONE', #702, #8500, #2952, .T. ) ;
#1227 = CARTESIAN_POINT ( 'NONE',  ( 303.3333333333333144, -20.00000000000000000, 165.1500000000000625 ) ) ;
#1228 = DIRECTION ( 'NONE',  ( -0.000000000000000000, 1.000000000000000000, -0.000000000000000000 ) ) ;
#1229 = CARTESIAN_POINT ( 'NONE',  ( 0.000000000000000000, 0.000000000000000000, 140.0000000000000000 ) ) ;
#1230 = AXIS2_PLACEMENT_3D ( 'NONE', #2656, #5257, #6524 ) ;
#1231 = CARTESIAN_POINT ( 'NONE',  ( -5.000000000000001776, 5.000000000000001776, -135.0000000000000000 ) ) ;
#1232 = DIRECTION ( 'NONE',  ( -0.7071067811865306973, 0.000000000000000000, 0.7071067811865643371 ) ) ;
#1233 = EDGE_CURVE ( 'NONE', #5259, #66, #3566, .T. ) ;
#1234 = CIRCLE ( 'NONE', #3737, 10.00000000000000000 ) ;
#1235 = CARTESIAN_POINT ( 'NONE',  ( -2.499999999999999556, 3.061616997868382648E-16, 3.469446951953614189E-15 ) ) ;
#1236 = LINE ( 'NONE', #1279, #1910 ) ;
#1237 = EDGE_LOOP ( 'NONE', ( #2489, #3495, #7845, #8047 ) ) ;
#1238 = SURFACE_STYLE_USAGE ( .BOTH. , #3817 ) ;
#1239 = DIRECTION ( 'NONE',  ( 0.000000000000000000, -1.000000000000000000, 1.471414886128461471E-15 ) ) ;
#1240 = ORIENTED_EDGE ( 'NONE', *, *, #4828, .T. ) ;
#1241 =( REPRESENTATION_RELATIONSHIP ('NONE','NONE', #3312, #7686 ) REPRESENTATION_RELATIONSHIP_WITH_TRANSFORMATION ( #6381 )SHAPE_REPRESENTATION_RELATIONSHIP( ) );
#1242 = DIRECTION ( 'NONE',  ( 0.000000000000000000, 1.000000000000000000, 0.000000000000000000 ) ) ;
#1243 = VECTOR ( 'NONE', #4493, 1000.000000000000000 ) ;
#1244 = EDGE_CURVE ( 'NONE', #238, #4249, #5603, .T. ) ;
#1245 = CARTESIAN_POINT ( 'NONE',  ( -5.000000000000000000, -5.000000000000000000, 148.0000000000000284 ) ) ;
#1246 = PRODUCT_DEFINITION_CONTEXT ( 'detailed design', #179, 'design' ) ;
#1247 = LINE ( 'NONE', #3956, #2037 ) ;
#1248 = VERTEX_POINT ( 'NONE', #6169 ) ;
#1249 = LINE ( 'NONE', #3908, #3655 ) ;
#1250 = CIRCLE ( 'NONE', #2379, 0.2500000000000002220 ) ;
#1251 = DIRECTION ( 'NONE',  ( -0.000000000000000000, 1.000000000000000000, -0.000000000000000000 ) ) ;
#1252 = ORIENTED_EDGE ( 'NONE', *, *, #5282, .T. ) ;
#1253 = ORIENTED_EDGE ( 'NONE', *, *, #2700, .T. ) ;
#1254 = CARTESIAN_POINT ( 'NONE',  ( -10.00000000000000000, 1.224646799147353256E-15, -97.99999999999997158 ) ) ;
#1255 = LINE ( 'NONE', #7967, #2443 ) ;
#1256 = CARTESIAN_POINT ( 'NONE',  ( 4.000000000000000000, -0.8732470631449981147, -3.223155494240760088 ) ) ;
#1257 = DIRECTION ( 'NONE',  ( 0.000000000000000000, -0.000000000000000000, -1.000000000000000000 ) ) ;
#1258 = VERTEX_POINT ( 'NONE', #3524 ) ;
#1259 = ORIENTED_EDGE ( 'NONE', *, *, #1007, .T. ) ;
#1260 = DIRECTION ( 'NONE',  ( -1.000000000000000000, 0.000000000000000000, -0.000000000000000000 ) ) ;
#1261 = EDGE_CURVE ( 'NONE', #5979, #7074, #6906, .T. ) ;
#1262 = AXIS2_PLACEMENT_3D ( 'NONE', #4433, #3134, #426 ) ;
#1263 = EDGE_CURVE ( 'NONE', #1874, #8118, #8146, .T. ) ;
#1264 = FACE_BOUND ( 'NONE', #2961, .T. ) ;
#1265 = LINE ( 'NONE', #3928, #5668 ) ;
#1266 = EDGE_LOOP ( 'NONE', ( #5909, #963, #5140, #6871 ) ) ;
#1267 = CARTESIAN_POINT ( 'NONE',  ( 10.00000000000000000, 0.000000000000000000, 120.0000000000000142 ) ) ;
#1268 = DIRECTION ( 'NONE',  ( -0.000000000000000000, -0.000000000000000000, 1.000000000000000000 ) ) ;
#1269 = CARTESIAN_POINT ( 'NONE',  ( 2.500000000000000000, 2.357898499370433054, -1.951563910473907981E-15 ) ) ;
#1270 = PRODUCT ( 'hex flange nut gradea_iso_ISO - 4161 - M5 - N', 'hex flange nut gradea_iso_ISO - 4161 - M5 - N', '', ( #4162 ) ) ;
#1271 = LINE ( 'NONE', #621, #8385 ) ;
#1272 = AXIS2_PLACEMENT_3D ( 'NONE', #496, #1855, #2511 ) ;
#1273 = CARTESIAN_POINT ( 'NONE',  ( 5.000000000000000000, -5.000000000000000000, 148.0000000000000284 ) ) ;
#1274 = PLANE ( 'NONE',  #7841 ) ;
#1275 = DIRECTION ( 'NONE',  ( 0.000000000000000000, 0.000000000000000000, 1.000000000000000000 ) ) ;
#1276 = EDGE_CURVE ( 'NONE', #2983, #951, #203, .T. ) ;
#1277 = CIRCLE ( 'NONE', #6137, 20.00000000000000000 ) ;
#1278 = DIRECTION ( 'NONE',  ( 0.000000000000000000, 0.000000000000000000, 1.000000000000000000 ) ) ;
#1279 = CARTESIAN_POINT ( 'NONE',  ( 82.99999999999998579, -4.999999999999998224, 145.0000000000000284 ) ) ;
#1280 = VERTEX_POINT ( 'NONE', #8187 ) ;
#1281 = VECTOR ( 'NONE', #1939, 1000.000000000000000 ) ;
#1282 = DIRECTION ( 'NONE',  ( -0.000000000000000000, -0.000000000000000000, 1.000000000000000000 ) ) ;
#1283 = ORIENTED_EDGE ( 'NONE', *, *, #5388, .F. ) ;
#1284 = CARTESIAN_POINT ( 'NONE',  ( 4.000000000000000000, 2.309401076758497151, -3.433295621305379353 ) ) ;
#1285 = AXIS2_PLACEMENT_3D ( 'NONE', #7939, #6622, #1975 ) ;
#1286 = CARTESIAN_POINT ( 'NONE',  ( 219.9999999999999716, -14.99999999999999822, 159.8500000000001080 ) ) ;
#1287 = VECTOR ( 'NONE', #2042, 1000.000000000000000 ) ;
#1288 = VECTOR ( 'NONE', #820, 1000.000000000000000 ) ;
#1289 = LINE ( 'NONE', #7341, #1064 ) ;
#1290 = EDGE_LOOP ( 'NONE', ( #5691, #2012 ) ) ;
#1291 = AXIS2_PLACEMENT_3D ( 'NONE', #4138, #3489, #161 ) ;
#1292 = CARTESIAN_POINT ( 'NONE',  ( 219.9999999999999716, -20.00000000000000000, 162.5000000000000853 ) ) ;
#1293 = DIRECTION ( 'NONE',  ( 6.123233985217515406E-17, -1.000000000000000000, -2.214089701702311143E-25 ) ) ;
#1294 = CARTESIAN_POINT ( 'NONE',  ( 0.000000000000000000, 0.000000000000000000, 145.0000000000000284 ) ) ;
#1295 = EDGE_LOOP ( 'NONE', ( #4425, #5553, #1036, #7577, #5292, #7395 ) ) ;
#1296 = AXIS2_PLACEMENT_3D ( 'NONE', #1245, #4547, #6634 ) ;
#1297 = ORIENTED_EDGE ( 'NONE', *, *, #3064, .T. ) ;
#1298 = DIRECTION ( 'NONE',  ( 0.000000000000000000, 0.000000000000000000, -1.000000000000000000 ) ) ;
#1299 = DIRECTION ( 'NONE',  ( 0.000000000000000000, 0.000000000000000000, 1.000000000000000000 ) ) ;
#1300 = EDGE_CURVE ( 'NONE', #7097, #1468, #7100, .T. ) ;
#1301 = EDGE_CURVE ( 'NONE', #1635, #478, #7525, .T. ) ;
#1302 = AXIS2_PLACEMENT_3D ( 'NONE', #5543, #5456, #8086 ) ;
#1303 = DIRECTION ( 'NONE',  ( 0.000000000000000000, 0.000000000000000000, 1.000000000000000000 ) ) ;
#1304 = CARTESIAN_POINT ( 'NONE',  ( 10.00000000000000000, 0.000000000000000000, 120.0000000000000000 ) ) ;
#1305 = ORIENTED_EDGE ( 'NONE', *, *, #6099, .F. ) ;
#1306 = EDGE_CURVE ( 'NONE', #4697, #6157, #1633, .T. ) ;
#1307 = ORIENTED_EDGE ( 'NONE', *, *, #88, .F. ) ;
#1308 = CARTESIAN_POINT ( 'NONE',  ( 20.00000000000000000, 0.000000000000000000, -49.56854249492377562 ) ) ;
#1309 = AXIS2_PLACEMENT_3D ( 'NONE', #5172, #1051, #4439 ) ;
#1310 = FACE_BOUND ( 'NONE', #5483, .T. ) ;
#1311 = LINE ( 'NONE', #7982, #7625 ) ;
#1312 = EDGE_LOOP ( 'NONE', ( #195, #5054, #7974, #2811, #739 ) ) ;
#1313 = CARTESIAN_POINT ( 'NONE',  ( 259.0000000000000000, -4.999999999999998224, 145.0000000000000284 ) ) ;
#1314 = SURFACE_STYLE_USAGE ( .BOTH. , #7192 ) ;
#1315 = EDGE_CURVE ( 'NONE', #7355, #5816, #3886, .T. ) ;
#1316 = CARTESIAN_POINT ( 'NONE',  ( 181.0000000000000000, 5.000000000000000000, 145.0000000000000284 ) ) ;
#1317 = DIRECTION ( 'NONE',  ( 1.000000000000000000, 0.000000000000000000, -0.000000000000000000 ) ) ;
#1318 = LINE ( 'NONE', #1360, #3234 ) ;
#1319 = CARTESIAN_POINT ( 'NONE',  ( 0.000000000000000000, 0.000000000000000000, -0.3080913168122742518 ) ) ;
#1320 = CARTESIAN_POINT ( 'NONE',  ( 303.3333333333333144, -20.00000000000000000, 162.5000000000000853 ) ) ;
#1321 = CARTESIAN_POINT ( 'NONE',  ( 25.00000000000000000, 0.000000000000000000, 2.055000000000000160 ) ) ;
#1322 = ORIENTED_EDGE ( 'NONE', *, *, #4702, .F. ) ;
#1323 = AXIS2_PLACEMENT_3D ( 'NONE', #7092, #3181, #3705 ) ;
#1324 = VERTEX_POINT ( 'NONE', #5645 ) ;
#1325 = EDGE_LOOP ( 'NONE', ( #7906, #6774 ) ) ;
#1326 = DIRECTION ( 'NONE',  ( -0.000000000000000000, 0.000000000000000000, -1.000000000000000000 ) ) ;
#1327 = CARTESIAN_POINT ( 'NONE',  ( 5.000000000000000000, -5.000000000000000000, 140.0000000000000000 ) ) ;
#1328 = AXIS2_PLACEMENT_3D ( 'NONE', #513, #7041, #3172 ) ;
#1329 = CLOSED_SHELL ( 'NONE', ( #2505, #7115, #8212, #480, #7684, #1352, #4698, #853, #2558, #1683, #6351, #7379, #3398, #3268, #2324, #900, #7472, #948, #5899, #2633 ) ) ;
#1330 = DIRECTION ( 'NONE',  ( -0.000000000000000000, 0.000000000000000000, 1.000000000000000000 ) ) ;
#1331 = ORIENTED_EDGE ( 'NONE', *, *, #6988, .T. ) ;
#1332 = CARTESIAN_POINT ( 'NONE',  ( -10.00000000000000000, 1.224646799147353256E-15, 120.0000000000000000 ) ) ;
#1333 = CARTESIAN_POINT ( 'NONE',  ( 0.000000000000000000, 0.000000000000000000, 62.00000000000001421 ) ) ;
#1334 = DIRECTION ( 'NONE',  ( 6.123233995736766036E-17, -1.000000000000000000, 0.000000000000000000 ) ) ;
#1335 = CARTESIAN_POINT ( 'NONE',  ( 219.9999999999999716, -15.00000000000000000, 162.5000000000000853 ) ) ;
#1336 = ORIENTED_EDGE ( 'NONE', *, *, #1493, .T. ) ;
#1337 = VERTEX_POINT ( 'NONE', #5037 ) ;
#1339 = AXIS2_PLACEMENT_3D ( 'NONE', #5714, #7733, #452 ) ;
#1338 = FACE_OUTER_BOUND ( 'NONE', #4464, .T. ) ;
#1340 = PLANE ( 'NONE',  #6168 ) ;
#1341 = ADVANCED_FACE ( 'NONE', ( #1126 ), #3869, .F. ) ;
#1342 =( GEOMETRIC_REPRESENTATION_CONTEXT ( 3 ) GLOBAL_UNCERTAINTY_ASSIGNED_CONTEXT ( ( #4950 ) ) GLOBAL_UNIT_ASSIGNED_CONTEXT ( ( #405, #2467, #447 ) ) REPRESENTATION_CONTEXT ( 'NONE', 'WORKASPACE' ) );
#1343 = DIRECTION ( 'NONE',  ( 0.000000000000000000, 0.000000000000000000, 1.000000000000000000 ) ) ;
#1344 = AXIS2_PLACEMENT_3D ( 'NONE', #2621, #6085, #6001 ) ;
#1345 = PRODUCT_DEFINITION_SHAPE ( 'NONE', 'NONE',  #7229 ) ;
#1346 = CARTESIAN_POINT ( 'NONE',  ( 352.0000000000000000, -20.00000000000000000, -16.23142504031546807 ) ) ;
#1347 = ORIENTED_EDGE ( 'NONE', *, *, #6080, .F. ) ;
#1348 = EDGE_CURVE ( 'NONE', #4522, #2939, #1041, .T. ) ;
#1349 = EDGE_LOOP ( 'NONE', ( #3392, #4034, #1184, #4779 ) ) ;
#1350 = CARTESIAN_POINT ( 'NONE',  ( 0.1750025118121568690, 4.719839900820621104, -3.469254087858248070 ) ) ;
#1351 = EDGE_CURVE ( 'NONE', #392, #596, #1921, .T. ) ;
#1352 = ADVANCED_FACE ( 'NONE', ( #4429 ), #1696, .F. ) ;
#1353 = DIRECTION ( 'NONE',  ( 0.000000000000000000, 0.000000000000000000, 1.000000000000000000 ) ) ;
#1354 = CARTESIAN_POINT ( 'NONE',  ( 5.000000000000000000, 5.000000000000000000, -105.9999999999999858 ) ) ;
#1355 = ORIENTED_EDGE ( 'NONE', *, *, #776, .T. ) ;
#1356 = LINE ( 'NONE', #3320, #6389 ) ;
#1357 =( REPRESENTATION_RELATIONSHIP ('NONE','NONE', #3312, #1479 ) REPRESENTATION_RELATIONSHIP_WITH_TRANSFORMATION ( #2393 )SHAPE_REPRESENTATION_RELATIONSHIP( ) );
#1358 = LINE ( 'NONE', #7366, #1980 ) ;
#1359 = FACE_OUTER_BOUND ( 'NONE', #4254, .T. ) ;
#1360 = CARTESIAN_POINT ( 'NONE',  ( 444.9999999999999432, -4.999999999999998224, 140.0000000000000000 ) ) ;
#1361 = LINE ( 'NONE', #4625, #8352 ) ;
#1362 = CARTESIAN_POINT ( 'NONE',  ( 82.99999999999998579, -4.999999999999998224, 140.0000000000000000 ) ) ;
#1363 = LINE ( 'NONE', #3985, #3019 ) ;
#1364 = CIRCLE ( 'NONE', #3460, 2.649999999999985700 ) ;
#1365 = ORIENTED_EDGE ( 'NONE', *, *, #1460, .T. ) ;
#1366 = SURFACE_STYLE_FILL_AREA ( #7334 ) ;
#1367 = VERTEX_POINT ( 'NONE', #3779 ) ;
#1368 = ITEM_DEFINED_TRANSFORMATION ( 'NONE', 'NONE', #3087,  #594 ) ;
#1369 = UNCERTAINTY_MEASURE_WITH_UNIT (LENGTH_MEASURE( 1.000000000000000082E-05 ), #4293, 'distance_accuracy_value', 'NONE');
#1370 = ORIENTED_EDGE ( 'NONE', *, *, #1684, .T. ) ;
#1371 = DIRECTION ( 'NONE',  ( 0.000000000000000000, 0.000000000000000000, 1.000000000000000000 ) ) ;
#1372 = CARTESIAN_POINT ( 'NONE',  ( 1.734723475976807094E-15, 4.618802153517012954, -0.4999999999999995559 ) ) ;
#1373 = VECTOR ( 'NONE', #7481, 1000.000000000000000 ) ;
#1374 = EDGE_CURVE ( 'NONE', #1123, #951, #3693, .T. ) ;
#1375 = EDGE_CURVE ( 'NONE', #4726, #7555, #7127, .T. ) ;
#1376 = EDGE_LOOP ( 'NONE', ( #713, #2858, #5114, #8177 ) ) ;
#1377 = DIRECTION ( 'NONE',  ( 1.000000000000000000, 0.000000000000000000, 0.000000000000000000 ) ) ;
#1378 = ORIENTED_EDGE ( 'NONE', *, *, #7017, .T. ) ;
#1379 = DIRECTION ( 'NONE',  ( 0.000000000000000000, 0.000000000000000000, -1.000000000000000000 ) ) ;
#1380 = EDGE_CURVE ( 'NONE', #2207, #5505, #6471, .T. ) ;
#1381 = DIRECTION ( 'NONE',  ( 0.000000000000000000, 0.000000000000000000, 1.000000000000000000 ) ) ;
#1382 = CIRCLE ( 'NONE', #687, 10.00000000000000000 ) ;
#1383 = APPLICATION_PROTOCOL_DEFINITION ( 'draft international standard', 'automotive_design', 1998, #2251 ) ;
#1384 = CARTESIAN_POINT ( 'NONE',  ( -5.000000000000001776, 5.000000000000001776, -27.99999999999999645 ) ) ;
#1385 = ORIENTED_EDGE ( 'NONE', *, *, #1994, .T. ) ;
#1386 = ORIENTED_EDGE ( 'NONE', *, *, #1213, .T. ) ;
#1387 = CARTESIAN_POINT ( 'NONE',  ( 25.00000000000000000, 2.055000000000000160, 0.000000000000000000 ) ) ;
#1388 = CARTESIAN_POINT ( 'NONE',  ( 352.0000000000000000, -25.00000000000000000, -13.58142504031548192 ) ) ;
#1389 = AXIS2_PLACEMENT_3D ( 'NONE', #4237, #6889, #4146 ) ;
#1390 = DIRECTION ( 'NONE',  ( 1.734723475976807587E-16, 1.000000000000000000, 0.000000000000000000 ) ) ;
#1391 = FACE_BOUND ( 'NONE', #1349, .T. ) ;
#1392 = EDGE_CURVE ( 'NONE', #4980, #798, #8360, .T. ) ;
#1393 = ORIENTED_EDGE ( 'NONE', *, *, #4033, .T. ) ;
#1394 = EDGE_LOOP ( 'NONE', ( #4253, #277, #2109, #1643 ) ) ;
#1395 = VECTOR ( 'NONE', #6494, 1000.000000000000000 ) ;
#1396 = CARTESIAN_POINT ( 'NONE',  ( 0.02448733951239481094, 4.877042772274728044, -3.751161874094022242 ) ) ;
#1397 = DIRECTION ( 'NONE',  ( 0.000000000000000000, -1.000000000000000000, 0.000000000000000000 ) ) ;
#1398 = CARTESIAN_POINT ( 'NONE',  ( -5.000000000000000000, -5.000000000000000000, -105.9999999999999858 ) ) ;
#1399 = VERTEX_POINT ( 'NONE', #7708 ) ;
#1400 = FACE_BOUND ( 'NONE', #6464, .T. ) ;
#1401 = EDGE_CURVE ( 'NONE', #3609, #917, #3778, .T. ) ;
#1402 = DIRECTION ( 'NONE',  ( 0.000000000000000000, 0.000000000000000000, -1.000000000000000000 ) ) ;
#1403 = LINE ( 'NONE', #8079, #4480 ) ;
#1404 = CARTESIAN_POINT ( 'NONE',  ( 352.0000000000000000, -20.00000000000000000, -16.23142504031546807 ) ) ;
#1405 = EDGE_CURVE ( 'NONE', #3511, #5594, #71, .T. ) ;
#1406 = CARTESIAN_POINT ( 'NONE',  ( 470.0000000000000000, 15.00000000000000000, 140.0000000000000000 ) ) ;
#1407 = DIRECTION ( 'NONE',  ( -0.000000000000000000, -0.000000000000000000, 1.000000000000000000 ) ) ;
#1408 =( GEOMETRIC_REPRESENTATION_CONTEXT ( 3 ) GLOBAL_UNCERTAINTY_ASSIGNED_CONTEXT ( ( #3074 ) ) GLOBAL_UNIT_ASSIGNED_CONTEXT ( ( #3269, #4564, #7927 ) ) REPRESENTATION_CONTEXT ( 'NONE', 'WORKASPACE' ) );
#1409 = EDGE_LOOP ( 'NONE', ( #2213, #1591 ) ) ;
#1410 = EDGE_CURVE ( 'NONE', #832, #4980, #4398, .T. ) ;
#1411 = ORIENTED_EDGE ( 'NONE', *, *, #8314, .T. ) ;
#1412 = EDGE_LOOP ( 'NONE', ( #1000, #1132, #7088, #5511 ) ) ;
#1413 = CARTESIAN_POINT ( 'NONE',  ( 434.9999999999999432, 5.000000000000001776, 139.9990000000000236 ) ) ;
#1414 = SURFACE_STYLE_USAGE ( .BOTH. , #7463 ) ;
#1415 = AXIS2_PLACEMENT_3D ( 'NONE', #64, #2608, #4040 ) ;
#1416 = PRODUCT_DEFINITION_SHAPE ( 'NONE', 'NONE',  #7502 ) ;
#1417 = COLOUR_RGB ( '',0.8941176470588234615, 0.8941176470588234615, 0.8941176470588234615 ) ;
#1418 = ORIENTED_EDGE ( 'NONE', *, *, #8394, .F. ) ;
#1419 = DIRECTION ( 'NONE',  ( 0.000000000000000000, 0.000000000000000000, 1.000000000000000000 ) ) ;
#1420 = AXIS2_PLACEMENT_3D ( 'NONE', #2139, #4833, #5521 ) ;
#1421 = ORIENTED_EDGE ( 'NONE', *, *, #7067, .T. ) ;
#1422 = DIRECTION ( 'NONE',  ( 0.000000000000000000, 0.000000000000000000, -1.000000000000000000 ) ) ;
#1423 = PLANE ( 'NONE',  #5781 ) ;
#1424 = AXIS2_PLACEMENT_3D ( 'NONE', #3135, #8322, #6436 ) ;
#1425 = PRODUCT_CONTEXT ( 'NONE', #2585, 'mechanical' ) ;
#1426 = VERTEX_POINT ( 'NONE', #3735 ) ;
#1427 = VECTOR ( 'NONE', #7633, 1000.000000000000000 ) ;
#1428 = VERTEX_POINT ( 'NONE', #5728 ) ;
#1429 = ADVANCED_FACE ( 'NONE', ( #8407 ), #2446, .F. ) ;
#1430 = CARTESIAN_POINT ( 'NONE',  ( -31.74999999999995737, 5.204748896376250699E-16, -4.250000000000000000 ) ) ;
#1431 = DIRECTION ( 'NONE',  ( -0.000000000000000000, 1.000000000000000000, -0.000000000000000000 ) ) ;
#1432 = CIRCLE ( 'NONE', #3936, 4.000000000000000000 ) ;
#1433 = AXIS2_PLACEMENT_3D ( 'NONE', #6787, #210, #964 ) ;
#1434 = CARTESIAN_POINT ( 'NONE',  ( 1.317756351988342622, -3.857995168970215438, -0.04852650426602527628 ) ) ;
#1435 = CARTESIAN_POINT ( 'NONE',  ( 3.510273485745307731, 2.827716139362654424, -3.610536846335885564 ) ) ;
#1436 = ORIENTED_EDGE ( 'NONE', *, *, #4897, .F. ) ;
#1437 = VECTOR ( 'NONE', #5283, 1000.000000000000000 ) ;
#1438 = FACE_OUTER_BOUND ( 'NONE', #2297, .T. ) ;
#1439 = VERTEX_POINT ( 'NONE', #2688 ) ;
#1440 = ORIENTED_EDGE ( 'NONE', *, *, #6089, .T. ) ;
#1441 = CARTESIAN_POINT ( 'NONE',  ( 170.9999999999999716, 5.000000000000001776, 145.0000000000000284 ) ) ;
#1442 = AXIS2_PLACEMENT_3D ( 'NONE', #2110, #4768, #809 ) ;
#1443 = B_SPLINE_CURVE_WITH_KNOTS ( 'NONE', 3,
 ( #8284, #4878, #4791, #118, #7400, #2790, #4101, #2142 ),
 .UNSPECIFIED., .F., .F.,
 ( 4, 2, 2, 4 ),
 ( 2.465131517071352357E-07, 0.001183067374689843057, 0.001774477805458910071, 0.002365888236227977302 ),
 .UNSPECIFIED. ) ;
#1444 = CARTESIAN_POINT ( 'NONE',  ( 0.000000000000000000, 0.000000000000000000, 148.0000000000000284 ) ) ;
#1445 = FACE_OUTER_BOUND ( 'NONE', #6630, .T. ) ;
#1446 = EDGE_LOOP ( 'NONE', ( #4645, #2394, #6555, #7740 ) ) ;
#1447 = CARTESIAN_POINT ( 'NONE',  ( 5.000000000000000000, -5.000000000000000000, -27.99999999999999645 ) ) ;
#1448 = VECTOR ( 'NONE', #1962, 1000.000000000000000 ) ;
#1449 = LINE ( 'NONE', #4887, #2264 ) ;
#1450 = FACE_OUTER_BOUND ( 'NONE', #2004, .T. ) ;
#1451 = CARTESIAN_POINT ( 'NONE',  ( 136.6666666666666288, -20.00000000000000000, 165.1500000000000625 ) ) ;
#1452 = DIRECTION ( 'NONE',  ( 0.9396926207859138680, 1.150791560227856926E-16, -0.3420201433256536139 ) ) ;
#1453 = ORIENTED_EDGE ( 'NONE', *, *, #7637, .F. ) ;
#1454 = EDGE_CURVE ( 'NONE', #5984, #4522, #3386, .T. ) ;
#1455 = ORIENTED_EDGE ( 'NONE', *, *, #6019, .F. ) ;
#1456 = EDGE_CURVE ( 'NONE', #7186, #4028, #5849, .T. ) ;
#1457 = ORIENTED_EDGE ( 'NONE', *, *, #2206, .T. ) ;
#1458 = CARTESIAN_POINT ( 'NONE',  ( 439.9999999999999432, -20.00000000000000000, 18.96857495968446017 ) ) ;
#1459 = ADVANCED_FACE ( 'NONE', ( #595 ), #5978, .F. ) ;
#1460 = EDGE_CURVE ( 'NONE', #917, #5858, #1247, .T. ) ;
#1461 = ORIENTED_EDGE ( 'NONE', *, *, #850, .T. ) ;
#1462 = CARTESIAN_POINT ( 'NONE',  ( 53.33333333333330017, -25.00000000000000000, 165.1500000000000625 ) ) ;
#1463 = EDGE_LOOP ( 'NONE', ( #5434, #8450, #5094, #893 ) ) ;
#1464 = DIRECTION ( 'NONE',  ( -0.000000000000000000, -0.000000000000000000, -1.000000000000000000 ) ) ;
#1465 = DIRECTION ( 'NONE',  ( -1.000000000000000000, 0.000000000000000000, 0.000000000000000000 ) ) ;
#1466 = DIRECTION ( 'NONE',  ( 0.000000000000000000, -1.000000000000000000, 0.000000000000000000 ) ) ;
#1467 = ORIENTED_EDGE ( 'NONE', *, *, #7367, .F. ) ;
#1468 = VERTEX_POINT ( 'NONE', #4896 ) ;
#1469 = LINE ( 'NONE', #8144, #2419 ) ;
#1470 = CARTESIAN_POINT ( 'NONE',  ( 2.500000000000000000, 0.000000000000000000, 0.000000000000000000 ) ) ;
#1471 = AXIS2_PLACEMENT_3D ( 'NONE', #2548, #5905, #72 ) ;
#1472 = CARTESIAN_POINT ( 'NONE',  ( 434.9999999999999432, -4.999999999999998224, 140.0000000000000000 ) ) ;
#1473 = ADVANCED_FACE ( 'NONE', ( #2644 ), #6548, .F. ) ;
#1474 = CARTESIAN_POINT ( 'NONE',  ( -0.1404048886732797152, -4.699864953788083888, -3.686887068327043160 ) ) ;
#1475 = ORIENTED_EDGE ( 'NONE', *, *, #3348, .T. ) ;
#1476 = ADVANCED_BREP_SHAPE_REPRESENTATION ( '', ( #2129, #594 ), #4077 ) ;
#1477 = AXIS2_PLACEMENT_3D ( 'NONE', #3255, #4683, #5896 ) ;
#1478 = CLOSED_SHELL ( 'NONE', ( #4062, #4552, #4311, #4235, #4388, #4568, #5994, #3402, #6076, #8173, #132, #3939, #6835, #4648, #3541, #482, #2530, #6537, #2671, #3502 ) ) ;
#1479 = SHAPE_REPRESENTATION ( 'socket head cap screw_iso_ISO 4762 M5 x 20 - 20N', ( #594 ), #5323 ) ;
#1480 = CARTESIAN_POINT ( 'NONE',  ( 0.000000000000000000, 0.000000000000000000, 0.000000000000000000 ) ) ;
#1481 = DIRECTION ( 'NONE',  ( -0.000000000000000000, -0.000000000000000000, 1.000000000000000000 ) ) ;
#1482 = ORIENTED_EDGE ( 'NONE', *, *, #2411, .T. ) ;
#1483 = ORIENTED_EDGE ( 'NONE', *, *, #508, .F. ) ;
#1484 = CARTESIAN_POINT ( 'NONE',  ( 4.999999999999997335, 135.0000000000000000, 25.00000000000000000 ) ) ;
#1485 = VECTOR ( 'NONE', #5322, 1000.000000000000000 ) ;
#1486 = CIRCLE ( 'NONE', #7458, 2.649999999999985700 ) ;
#1487 = LINE ( 'NONE', #6920, #5368 ) ;
#1488 = EDGE_CURVE ( 'NONE', #1985, #2428, #8577, .T. ) ;
#1489 = PLANE ( 'NONE',  #4705 ) ;
#1490 = VERTEX_POINT ( 'NONE', #5285 ) ;
#1491 = ADVANCED_FACE ( 'NONE', ( #1953 ), #6512, .T. ) ;
#1492 = CARTESIAN_POINT ( 'NONE',  ( 0.000000000000000000, 0.000000000000000000, 140.0000000000000000 ) ) ;
#1493 = EDGE_CURVE ( 'NONE', #1660, #542, #6479, .T. ) ;
#1494 = PRODUCT ( 'MAS-188', 'MAS-188', '', ( #3165 ) ) ;
#1495 = CARTESIAN_POINT ( 'NONE',  ( -2.682243648011671588, -3.070208061305317759, -0.04852650426602272971 ) ) ;
#1496 = DIRECTION ( 'NONE',  ( 1.000000000000000000, 1.734723475976806848E-16, -0.000000000000000000 ) ) ;
#1497 = CYLINDRICAL_SURFACE ( 'NONE', #1389, 4.250000000000000000 ) ;
#1498 = FACE_OUTER_BOUND ( 'NONE', #3641, .T. ) ;
#1499 = DIRECTION ( 'NONE',  ( 0.000000000000000000, 1.000000000000000000, 0.000000000000000000 ) ) ;
#1500 = ORIENTED_EDGE ( 'NONE', *, *, #5284, .F. ) ;
#1501 = VERTEX_POINT ( 'NONE', #549 ) ;
#1502 = ORIENTED_EDGE ( 'NONE', *, *, #981, .T. ) ;
#1503 = FACE_OUTER_BOUND ( 'NONE', #8063, .T. ) ;
#1504 = EDGE_CURVE ( 'NONE', #8019, #7048, #6892, .T. ) ;
#1505 = FILL_AREA_STYLE ('',( #98 ) ) ;
#1506 = VECTOR ( 'NONE', #6180, 1000.000000000000000 ) ;
#1507 = ORIENTED_EDGE ( 'NONE', *, *, #6503, .T. ) ;
#1508 = CARTESIAN_POINT ( 'NONE',  ( -5.384454397937118664, 6.594054843588581554E-16, -4.484454397937119197 ) ) ;
#1509 = EDGE_LOOP ( 'NONE', ( #1657, #6, #6723, #2905 ) ) ;
#1510 = CARTESIAN_POINT ( 'NONE',  ( 0.000000000000000000, 0.000000000000000000, -135.0000000000000000 ) ) ;
#1511 = FACE_OUTER_BOUND ( 'NONE', #5220, .T. ) ;
#1512 = PRODUCT_CONTEXT ( 'NONE', #2313, 'mechanical' ) ;
#1513 = PRESENTATION_STYLE_ASSIGNMENT (( #4733 ) ) ;
#1514 = VERTEX_POINT ( 'NONE', #639 ) ;
#1515 = EDGE_CURVE ( 'NONE', #7956, #6857, #4954, .T. ) ;
#1516 = ORIENTED_EDGE ( 'NONE', *, *, #6611, .T. ) ;
#1517 = CARTESIAN_POINT ( 'NONE',  ( -4.211140560182196957, -2.431303136016552013, -3.745885042887436178 ) ) ;
#1518 = AXIS2_PLACEMENT_3D ( 'NONE', #3204, #5235, #336 ) ;
#1519 = DIRECTION ( 'NONE',  ( 0.000000000000000000, 1.000000000000000000, 0.000000000000000000 ) ) ;
#1520 = CARTESIAN_POINT ( 'NONE',  ( -30.00000000000000000, 15.00000000000000000, 145.0000000000000284 ) ) ;
#1521 = DIRECTION ( 'NONE',  ( 0.000000000000000000, 0.000000000000000000, 1.000000000000000000 ) ) ;
#1522 = ORIENTED_EDGE ( 'NONE', *, *, #1652, .T. ) ;
#1523 = FILL_AREA_STYLE_COLOUR ( '', #6540 ) ;
#1524 = DIRECTION ( 'NONE',  ( -1.734723475976806848E-16, -1.000000000000000000, 0.000000000000000000 ) ) ;
#1525 = VERTEX_POINT ( 'NONE', #7247 ) ;
#1526 = EDGE_LOOP ( 'NONE', ( #1440, #3470, #992, #6874 ) ) ;
#1527 = CARTESIAN_POINT ( 'NONE',  ( 0.000000000000000000, 0.000000000000000000, 42.00000000000000711 ) ) ;
#1528 = DIRECTION ( 'NONE',  ( 0.000000000000000000, -0.000000000000000000, 1.000000000000000000 ) ) ;
#1529 =( REPRESENTATION_RELATIONSHIP ('NONE','NONE', #3312, #1479 ) REPRESENTATION_RELATIONSHIP_WITH_TRANSFORMATION ( #6206 )SHAPE_REPRESENTATION_RELATIONSHIP( ) );
#1530 = AXIS2_PLACEMENT_3D ( 'NONE', #3361, #7276, #664 ) ;
#1531 = CARTESIAN_POINT ( 'NONE',  ( 5.000000000000001776, -4.999999999999998224, 145.0000000000000284 ) ) ;
#1532 = DIRECTION ( 'NONE',  ( -1.000000000000000000, 0.000000000000000000, 0.000000000000000000 ) ) ;
#1533 = SHAPE_REPRESENTATION ( 'roller axis assy_r1', ( #594 ), #1167 ) ;
#1534 = ORIENTED_EDGE ( 'NONE', *, *, #3805, .T. ) ;
#1535 = DIRECTION ( 'NONE',  ( 0.000000000000000000, 0.5000000000000011102, 0.8660254037844380415 ) ) ;
#1536 = AXIS2_PLACEMENT_3D ( 'NONE', #2377, #2507, #7102 ) ;
#1537 = DIRECTION ( 'NONE',  ( 0.000000000000000000, 0.000000000000000000, 1.000000000000000000 ) ) ;
#1538 = EDGE_CURVE ( 'NONE', #1967, #3708, #8003, .T. ) ;
#1539 = EDGE_CURVE ( 'NONE', #6157, #4697, #2592, .T. ) ;
#1540 = CARTESIAN_POINT ( 'NONE',  ( 53.33333333333330017, -20.00000000000000000, 159.8500000000001080 ) ) ;
#1541 = CARTESIAN_POINT ( 'NONE',  ( -5.000000000000000000, -5.000000000000000000, 148.0000000000000284 ) ) ;
#1542 = LINE ( 'NONE', #3544, #3198 ) ;
#1543 = ORIENTED_EDGE ( 'NONE', *, *, #6736, .F. ) ;
#1544 = ORIENTED_EDGE ( 'NONE', *, *, #6214, .T. ) ;
#1545 = ORIENTED_EDGE ( 'NONE', *, *, #5785, .T. ) ;
#1546 = CARTESIAN_POINT ( 'NONE',  ( 0.000000000000000000, 0.000000000000000000, 0.000000000000000000 ) ) ;
#1547 = CARTESIAN_POINT ( 'NONE',  ( 470.0000000000000000, -20.00000000000000000, 180.0000000000000284 ) ) ;
#1548 = EDGE_CURVE ( 'NONE', #1426, #6694, #1289, .T. ) ;
#1549 = VERTEX_POINT ( 'NONE', #5244 ) ;
#1550 = DIRECTION ( 'NONE',  ( 0.000000000000000000, 1.000000000000000000, 0.000000000000000000 ) ) ;
#1551 = ORIENTED_EDGE ( 'NONE', *, *, #4510, .T. ) ;
#1552 = CYLINDRICAL_SURFACE ( 'NONE', #4351, 10.00000000000000000 ) ;
#1553 = CARTESIAN_POINT ( 'NONE',  ( -10.00000000000000000, 1.224646799147353256E-15, 120.0000000000000000 ) ) ;
#1554 = ITEM_DEFINED_TRANSFORMATION ( 'NONE', 'NONE', #138,  #594 ) ;
#1555 = CARTESIAN_POINT ( 'NONE',  ( 0.000000000000000000, 0.000000000000000000, 148.0000000000000284 ) ) ;
#1556 = VERTEX_POINT ( 'NONE', #59 ) ;
#1557 = EDGE_LOOP ( 'NONE', ( #1121, #7580, #6490, #5326, #2606 ) ) ;
#1558 = AXIS2_PLACEMENT_3D ( 'NONE', #4553, #5939, #6029 ) ;
#1559 = CARTESIAN_POINT ( 'NONE',  ( 470.0000000000000000, 15.00000000000000000, 145.0000000000000284 ) ) ;
#1560 = PRESENTATION_LAYER_ASSIGNMENT (  '', '', ( #5302 ) ) ;
#1561 = FACE_OUTER_BOUND ( 'NONE', #6059, .T. ) ;
#1562 = DIRECTION ( 'NONE',  ( 0.000000000000000000, 0.000000000000000000, -1.000000000000000000 ) ) ;
#1563 = PRODUCT_DEFINITION_SHAPE ( 'NONE', 'NONE',  #8615 ) ;
#1564 = CARTESIAN_POINT ( 'NONE',  ( 3.522875095019493141, -2.820352903225631369, -3.598441714920572299 ) ) ;
#1565 = VERTEX_POINT ( 'NONE', #4035 ) ;
#1566 = AXIS2_PLACEMENT_3D ( 'NONE', #2885, #4144, #4276 ) ;
#1567 = DIRECTION ( 'NONE',  ( -1.734723475976806848E-16, 1.000000000000000000, 0.000000000000000000 ) ) ;
#1568 = ORIENTED_EDGE ( 'NONE', *, *, #5736, .F. ) ;
#1569 = CONICAL_SURFACE ( 'NONE', #876, 2.059999999999998721, 0.9599310885968738161 ) ;
#1570 = ADVANCED_FACE ( 'NONE', ( #6676 ), #723, .F. ) ;
#1571 = CARTESIAN_POINT ( 'NONE',  ( 357.0000000000000000, -4.999999999999998224, 140.0000000000000000 ) ) ;
#1572 = DIRECTION ( 'NONE',  ( -1.734723475976806848E-16, 1.000000000000000000, 0.000000000000000000 ) ) ;
#1573 = EDGE_CURVE ( 'NONE', #542, #807, #4727, .T. ) ;
#1574 = CIRCLE ( 'NONE', #1291, 20.00000000000000000 ) ;
#1575 = EDGE_CURVE ( 'NONE', #4726, #2056, #1912, .T. ) ;
#1576 = MECHANICAL_DESIGN_GEOMETRIC_PRESENTATION_REPRESENTATION (  '', ( #7272 ), #887 ) ;
#1577 = VECTOR ( 'NONE', #6770, 1000.000000000000000 ) ;
#1578 = CARTESIAN_POINT ( 'NONE',  ( 2.500000000000000000, 3.004629197474318851E-15, 2.042000000000000259 ) ) ;
#1579 = FACE_OUTER_BOUND ( 'NONE', #2274, .T. ) ;
#1580 = EDGE_LOOP ( 'NONE', ( #2944, #1732, #5125, #1177 ) ) ;
#1581 = LINE ( 'NONE', #6883, #6243 ) ;
#1582 = CARTESIAN_POINT ( 'NONE',  ( 219.9999999999999716, -20.00000000000000000, 162.5000000000000853 ) ) ;
#1583 = AXIS2_PLACEMENT_3D ( 'NONE', #4984, #985, #1814 ) ;
#1584 = CARTESIAN_POINT ( 'NONE',  ( 0.000000000000000000, 0.000000000000000000, -4.484454397937119197 ) ) ;
#1585 = CARTESIAN_POINT ( 'NONE',  ( -5.000000000000001776, 5.000000000000001776, 148.0000000000000284 ) ) ;
#1586 = CARTESIAN_POINT ( 'NONE',  ( 3.679171394226031122, 2.494631558665830973, -0.3503314178412474389 ) ) ;
#1587 = CARTESIAN_POINT ( 'NONE',  ( 0.000000000000000000, 0.000000000000000000, -105.9999999999999858 ) ) ;
#1588 = CIRCLE ( 'NONE', #3253, 4.000000000000000000 ) ;
#1589 = EDGE_CURVE ( 'NONE', #8480, #6268, #75, .T. ) ;
#1590 = ORIENTED_EDGE ( 'NONE', *, *, #7756, .T. ) ;
#1591 = ORIENTED_EDGE ( 'NONE', *, *, #7360, .T. ) ;
#1592 = ORIENTED_EDGE ( 'NONE', *, *, #1759, .F. ) ;
#1593 = EDGE_CURVE ( 'NONE', #4392, #5678, #6106, .T. ) ;
#1594 = CARTESIAN_POINT ( 'NONE',  ( 0.000000000000000000, 0.000000000000000000, 62.00000000000001421 ) ) ;
#1595 = CONICAL_SURFACE ( 'NONE', #6455, 4.000000000000000000, 0.8911886515913786111 ) ;
#1596 = AXIS2_PLACEMENT_3D ( 'NONE', #4677, #591, #7163 ) ;
#1597 = ORIENTED_EDGE ( 'NONE', *, *, #1405, .T. ) ;
#1598 = DIRECTION ( 'NONE',  ( -1.000000000000000000, 0.000000000000000000, -0.000000000000000000 ) ) ;
#1599 = VERTEX_POINT ( 'NONE', #3598 ) ;
#1600 = DIRECTION ( 'NONE',  ( 1.000000000000000000, 0.000000000000000000, 0.000000000000000000 ) ) ;
#1601 = FACE_OUTER_BOUND ( 'NONE', #529, .T. ) ;
#1602 = EDGE_CURVE ( 'NONE', #1117, #6335, #4774, .T. ) ;
#1603 = ORIENTED_EDGE ( 'NONE', *, *, #1380, .T. ) ;
#1604 = EDGE_LOOP ( 'NONE', ( #4242, #1678 ) ) ;
#1605 = DIRECTION ( 'NONE',  ( 0.000000000000000000, 0.000000000000000000, 1.000000000000000000 ) ) ;
#1606 = CARTESIAN_POINT ( 'NONE',  ( 0.000000000000000000, 0.000000000000000000, -135.0000000000000000 ) ) ;
#1607 = DIRECTION ( 'NONE',  ( 0.000000000000000000, 0.000000000000000000, -1.000000000000000000 ) ) ;
#1608 = CARTESIAN_POINT ( 'NONE',  ( 2.804994570502171047, 3.229033611042449792, -3.526374918436834704 ) ) ;
#1609 = VERTEX_POINT ( 'NONE', #7426 ) ;
#1610 = LINE ( 'NONE', #7529, #2126 ) ;
#1611 = VERTEX_POINT ( 'NONE', #1462 ) ;
#1612 = AXIS2_PLACEMENT_3D ( 'NONE', #6869, #1607, #7617 ) ;
#1613 = CARTESIAN_POINT ( 'NONE',  ( -4.175648173966055587, 2.207990556236529844, -3.469390959564062626 ) ) ;
#1614 = LINE ( 'NONE', #256, #1882 ) ;
#1615 = ADVANCED_FACE ( 'NONE', ( #856 ), #5589, .F. ) ;
#1616 = VECTOR ( 'NONE', #2248, 1000.000000000000000 ) ;
#1617 = CARTESIAN_POINT ( 'NONE',  ( 2.500000000000000000, -1.178949249685213863, 2.042000000000002924 ) ) ;
#1618 = ADVANCED_FACE ( 'NONE', ( #7466 ), #7738, .T. ) ;
#1619 = AXIS2_PLACEMENT_3D ( 'NONE', #1333, #4777, #8096 ) ;
#1620 = DIRECTION ( 'NONE',  ( -0.000000000000000000, 1.000000000000000000, -0.000000000000000000 ) ) ;
#1621 = ORIENTED_EDGE ( 'NONE', *, *, #4246, .T. ) ;
#1622 = DIRECTION ( 'NONE',  ( 0.000000000000000000, 0.000000000000000000, -1.000000000000000000 ) ) ;
#1623 = ADVANCED_FACE ( 'NONE', ( #2205 ), #3011, .F. ) ;
#1624 = SHAPE_REPRESENTATION_RELATIONSHIP ( 'NONE' , 'NONE' ,  #4754, #759 ) ;
#1625 = CARTESIAN_POINT ( 'NONE',  ( -4.999999999999998224, 5.000000000000001776, 140.0000000000000000 ) ) ;
#1626 = EDGE_CURVE ( 'NONE', #428, #4949, #140, .T. ) ;
#1627 = CIRCLE ( 'NONE', #1070, 20.00000000000000000 ) ;
#1628 = CIRCLE ( 'NONE', #2739, 2.649999999999985700 ) ;
#1629 = FACE_BOUND ( 'NONE', #2134, .T. ) ;
#1630 = DIRECTION ( 'NONE',  ( 0.000000000000000000, 0.000000000000000000, 1.000000000000000000 ) ) ;
#1631 = DIRECTION ( 'NONE',  ( -0.000000000000000000, -0.000000000000000000, 1.000000000000000000 ) ) ;
#1632 = CARTESIAN_POINT ( 'NONE',  ( -5.000000000000001776, 5.000000000000001776, -27.99999999999999645 ) ) ;
#1633 = CIRCLE ( 'NONE', #1897, 10.00000000000000000 ) ;
#1634 = ORIENTED_EDGE ( 'NONE', *, *, #1964, .T. ) ;
#1635 = VERTEX_POINT ( 'NONE', #4857 ) ;
#1636 = EDGE_LOOP ( 'NONE', ( #1253, #4981 ) ) ;
#1637 = DIRECTION ( 'NONE',  ( -0.5000000000000051070, 1.060575238724903217E-16, -0.8660254037844355990 ) ) ;
#1638 = LINE ( 'NONE', #1727, #5607 ) ;
#1639 = PRODUCT_DEFINITION_SHAPE ( 'NONE', 'NONE',  #8627 ) ;
#1640 = ORIENTED_EDGE ( 'NONE', *, *, #5969, .F. ) ;
#1641 = CARTESIAN_POINT ( 'NONE',  ( -10.00000000000000000, 1.224646799147353256E-15, 140.0000000000000000 ) ) ;
#1642 = VECTOR ( 'NONE', #2175, 1000.000000000000000 ) ;
#1643 = ORIENTED_EDGE ( 'NONE', *, *, #3986, .T. ) ;
#1644 = SURFACE_SIDE_STYLE ('',( #3727 ) ) ;
#1645 = CARTESIAN_POINT ( 'NONE',  ( -4.999999999999998224, -4.999999999999998224, 139.9990000000000236 ) ) ;
#1646 = ITEM_DEFINED_TRANSFORMATION ( 'NONE', 'NONE', #4471,  #594 ) ;
#1647 = FILL_AREA_STYLE_COLOUR ( '', #1417 ) ;
#1648 = ORIENTED_EDGE ( 'NONE', *, *, #1351, .T. ) ;
#1649 = EDGE_LOOP ( 'NONE', ( #2501, #360, #4742 ) ) ;
#1650 = CARTESIAN_POINT ( 'NONE',  ( -4.207491450040567571, 2.029819825146470524, -3.671670828759566074 ) ) ;
#1651 = LINE ( 'NONE', #422, #5314 ) ;
#1652 = EDGE_CURVE ( 'NONE', #7956, #2382, #7598, .T. ) ;
#1653 = EDGE_CURVE ( 'NONE', #147, #5734, #945, .T. ) ;
#1654 = EDGE_CURVE ( 'NONE', #3461, #1123, #2900, .T. ) ;
#1655 = CARTESIAN_POINT ( 'NONE',  ( 386.6666666666666288, -20.00000000000000000, 165.1500000000000625 ) ) ;
#1656 = CARTESIAN_POINT ( 'NONE',  ( 386.6666666666666288, -14.99999999999999822, 165.1500000000000625 ) ) ;
#1657 = ORIENTED_EDGE ( 'NONE', *, *, #2296, .T. ) ;
#1658 = DIRECTION ( 'NONE',  ( 1.000000000000000000, 0.000000000000000000, 0.000000000000000000 ) ) ;
#1659 = DIRECTION ( 'NONE',  ( -1.000000000000000000, 1.734723475976807341E-16, -0.000000000000000000 ) ) ;
#1660 = VERTEX_POINT ( 'NONE', #7562 ) ;
#1661 = ORIENTED_EDGE ( 'NONE', *, *, #1043, .F. ) ;
#1662 = CARTESIAN_POINT ( 'NONE',  ( 0.000000000000000000, 157.5000000000000284, 5.000000000000000000 ) ) ;
#1663 = DIRECTION ( 'NONE',  ( -0.000000000000000000, 1.000000000000000000, -0.000000000000000000 ) ) ;
#1664 = AXIS2_PLACEMENT_3D ( 'NONE', #6665, #3369, #6585 ) ;
#1665 = ADVANCED_FACE ( 'NONE', ( #191 ), #2812, .T. ) ;
#1666 = DIRECTION ( 'NONE',  ( 1.000000000000000000, 0.000000000000000000, -0.000000000000000000 ) ) ;
#1667 = DIRECTION ( 'NONE',  ( 0.000000000000000000, 0.000000000000000000, -1.000000000000000000 ) ) ;
#1668 = ORIENTED_EDGE ( 'NONE', *, *, #6242, .F. ) ;
#1669 = CARTESIAN_POINT ( 'NONE',  ( 1.411581201560190495E-15, 4.862606272033091592, -3.745885042887436622 ) ) ;
#1670 = ORIENTED_EDGE ( 'NONE', *, *, #3587, .T. ) ;
#1671 = AXIS2_PLACEMENT_3D ( 'NONE', #7190, #1806, #2547 ) ;
#1672 = CYLINDRICAL_SURFACE ( 'NONE', #4610, 20.00000000000000000 ) ;
#1673 = DIRECTION ( 'NONE',  ( 1.000000000000000000, 1.734723475976806848E-16, 0.000000000000000000 ) ) ;
#1674 = AXIS2_PLACEMENT_3D ( 'NONE', #47, #3943, #3457 ) ;
#1675 = DIRECTION ( 'NONE',  ( -1.000000000000000000, 0.000000000000000000, 0.000000000000000000 ) ) ;
#1676 = CARTESIAN_POINT ( 'NONE',  ( -4.140404888673278272, -2.228338276487456415, -3.686887068327035166 ) ) ;
#1677 = CARTESIAN_POINT ( 'NONE',  ( -4.204114297095464359, 1.660363174096617156, -3.602136431857887011 ) ) ;
#1678 = ORIENTED_EDGE ( 'NONE', *, *, #953, .T. ) ;
#1679 = ORIENTED_EDGE ( 'NONE', *, *, #6271, .F. ) ;
#1680 = ORIENTED_EDGE ( 'NONE', *, *, #578, .F. ) ;
#1681 = CARTESIAN_POINT ( 'NONE',  ( 5.000000000000000000, 134.9989999999999952, 25.00000000000000000 ) ) ;
#1682 = LINE ( 'NONE', #3073, #8263 ) ;
#1683 = ADVANCED_FACE ( 'NONE', ( #8092 ), #3509, .T. ) ;
#1684 = EDGE_CURVE ( 'NONE', #4319, #6518, #3553, .T. ) ;
#1685 = ORIENTED_EDGE ( 'NONE', *, *, #6878, .T. ) ;
#1686 = DIRECTION ( 'NONE',  ( 0.000000000000000000, -1.000000000000000000, 0.000000000000000000 ) ) ;
#1687 = ORIENTED_EDGE ( 'NONE', *, *, #3454, .T. ) ;
#1688 = FILL_AREA_STYLE_COLOUR ( '', #462 ) ;
#1689 = DIRECTION ( 'NONE',  ( -1.000000000000000000, 0.000000000000000000, 0.000000000000000000 ) ) ;
#1690 = EDGE_LOOP ( 'NONE', ( #2075, #8055, #779, #8237 ) ) ;
#1691 = VERTEX_POINT ( 'NONE', #7608 ) ;
#1692 = LINE ( 'NONE', #5598, #7026 ) ;
#1693 = CARTESIAN_POINT ( 'NONE',  ( -5.000000000000001776, 5.000000000000001776, 148.0000000000000284 ) ) ;
#1694 =( GEOMETRIC_REPRESENTATION_CONTEXT ( 3 ) GLOBAL_UNCERTAINTY_ASSIGNED_CONTEXT ( ( #6372 ) ) GLOBAL_UNIT_ASSIGNED_CONTEXT ( ( #657, #2057, #697 ) ) REPRESENTATION_CONTEXT ( 'NONE', 'WORKASPACE' ) );
#1695 =( REPRESENTATION_RELATIONSHIP ('NONE','NONE', #3312, #1479 ) REPRESENTATION_RELATIONSHIP_WITH_TRANSFORMATION ( #3900 )SHAPE_REPRESENTATION_RELATIONSHIP( ) );
#1696 = PLANE ( 'NONE',  #919 ) ;
#1697 = DIRECTION ( 'NONE',  ( 0.000000000000000000, -1.000000000000000000, 0.000000000000000000 ) ) ;
#1698 = ORIENTED_EDGE ( 'NONE', *, *, #2070, .F. ) ;
#1699 = ADVANCED_FACE ( 'NONE', ( #2773 ), #2116, .F. ) ;
#1700 = PRODUCT_DEFINITION_FORMATION_WITH_SPECIFIED_SOURCE ( 'ANY', '', #654, .NOT_KNOWN. ) ;
#1701 = CARTESIAN_POINT ( 'NONE',  ( 352.0000000000000000, 0.000000000000000000, 0.000000000000000000 ) ) ;
#1702 = CARTESIAN_POINT ( 'NONE',  ( 5.000000000000000000, -5.000000000000000000, 140.0000000000000000 ) ) ;
#1703 = ORIENTED_EDGE ( 'NONE', *, *, #6279, .T. ) ;
#1704 = ORIENTED_EDGE ( 'NONE', *, *, #5473, .F. ) ;
#1705 = DIRECTION ( 'NONE',  ( 0.000000000000000000, 1.000000000000000000, 0.000000000000000000 ) ) ;
#1706 = LINE ( 'NONE', #7178, #5061 ) ;
#1707 = ORIENTED_EDGE ( 'NONE', *, *, #3455, .F. ) ;
#1708 = AXIS2_PLACEMENT_3D ( 'NONE', #6598, #4514, #7170 ) ;
#1709 = CARTESIAN_POINT ( 'NONE',  ( 0.000000000000000000, 1.178949249685213863, -2.042000000000001148 ) ) ;
#1710 = CARTESIAN_POINT ( 'NONE',  ( 0.000000000000000000, -15.00000000000000000, 0.000000000000000000 ) ) ;
#1711 = ORIENTED_EDGE ( 'NONE', *, *, #3167, .F. ) ;
#1712 = LINE ( 'NONE', #5660, #6937 ) ;
#1713 = VECTOR ( 'NONE', #2844, 1000.000000000000000 ) ;
#1714 =( LENGTH_UNIT ( ) NAMED_UNIT ( * ) SI_UNIT ( .MILLI., .METRE. ) );
#1715 = ORIENTED_EDGE ( 'NONE', *, *, #4826, .T. ) ;
#1716 = PRODUCT_DEFINITION_SHAPE ( 'NONE', 'NONE',  #8632 ) ;
#1717 = CARTESIAN_POINT ( 'NONE',  ( 136.6666666666666288, -25.00000000000000000, 159.8500000000001080 ) ) ;
#1718 = DIRECTION ( 'NONE',  ( 0.000000000000000000, 0.000000000000000000, 1.000000000000000000 ) ) ;
#1719 = AXIS2_PLACEMENT_3D ( 'NONE', #2690, #7168, #7912 ) ;
#1720 = DIRECTION ( 'NONE',  ( 1.000000000000000000, 0.000000000000000000, 0.000000000000000000 ) ) ;
#1721 = VECTOR ( 'NONE', #7839, 1000.000000000000000 ) ;
#1722 = DIRECTION ( 'NONE',  ( -1.000000000000000000, 0.000000000000000000, 0.000000000000000000 ) ) ;
#1723 = CARTESIAN_POINT ( 'NONE',  ( -4.211399284164270895, 2.459729995988205964, -3.751162237960538715 ) ) ;
#1724 = ORIENTED_EDGE ( 'NONE', *, *, #6796, .F. ) ;
#1725 = ORIENTED_EDGE ( 'NONE', *, *, #202, .T. ) ;
#1726 = LINE ( 'NONE', #454, #7000 ) ;
#1727 = CARTESIAN_POINT ( 'NONE',  ( 5.000000000000000000, 5.000000000000000000, 139.9990000000000236 ) ) ;
#1728 = AXIS2_PLACEMENT_3D ( 'NONE', #1546, #8132, #7462 ) ;
#1729 = ORIENTED_EDGE ( 'NONE', *, *, #5789, .F. ) ;
#1730 = SURFACE_SIDE_STYLE ('',( #370 ) ) ;
#1731 = EDGE_CURVE ( 'NONE', #2415, #6261, #2857, .T. ) ;
#1732 = ORIENTED_EDGE ( 'NONE', *, *, #3986, .F. ) ;
#1733 = DIRECTION ( 'NONE',  ( 1.000000000000000000, 0.000000000000000000, 0.000000000000000000 ) ) ;
#1734 = DIRECTION ( 'NONE',  ( -1.000000000000000000, 0.000000000000000000, 0.000000000000000000 ) ) ;
#1735 = EDGE_CURVE ( 'NONE', #807, #678, #3279, .T. ) ;
#1736 = ORIENTED_EDGE ( 'NONE', *, *, #7668, .T. ) ;
#1737 = ORIENTED_EDGE ( 'NONE', *, *, #6829, .F. ) ;
#1738 = VECTOR ( 'NONE', #431, 1000.000000000000000 ) ;
#1739 = CARTESIAN_POINT ( 'NONE',  ( 347.0000000000000000, 5.000000000000001776, 139.9990000000000236 ) ) ;
#1740 = EDGE_CURVE ( 'NONE', #1089, #3680, #4421, .T. ) ;
#1741 = CARTESIAN_POINT ( 'NONE',  ( 5.000000000000000000, -5.000000000000000000, 34.00000000000000711 ) ) ;
#1742 = CARTESIAN_POINT ( 'NONE',  ( 4.000000000000000000, -1.084202172485504434E-14, -3.142992957459231906 ) ) ;
#1743 = DIRECTION ( 'NONE',  ( 0.000000000000000000, 0.000000000000000000, 1.000000000000000000 ) ) ;
#1744 = ORIENTED_EDGE ( 'NONE', *, *, #1922, .F. ) ;
#1745 = DIRECTION ( 'NONE',  ( 1.000000000000000000, 0.000000000000000000, 0.000000000000000000 ) ) ;
#1746 = DIRECTION ( 'NONE',  ( 0.000000000000000000, 0.000000000000000000, 1.000000000000000000 ) ) ;
#1747 = VERTEX_POINT ( 'NONE', #6941 ) ;
#1748 = ORIENTED_EDGE ( 'NONE', *, *, #5809, .F. ) ;
#1749 = DIRECTION ( 'NONE',  ( -1.000000000000000000, 0.000000000000000000, 0.000000000000000000 ) ) ;
#1750 = DIRECTION ( 'NONE',  ( -0.000000000000000000, -1.000000000000000000, -0.000000000000000000 ) ) ;
#1751 = EDGE_CURVE ( 'NONE', #4177, #3374, #7031, .T. ) ;
#1752 = CARTESIAN_POINT ( 'NONE',  ( 176.0000000000000000, -20.00000000000000000, -89.28142504031545457 ) ) ;
#1753 = DIRECTION ( 'NONE',  ( 0.000000000000000000, 0.000000000000000000, 1.000000000000000000 ) ) ;
#1754 = VERTEX_POINT ( 'NONE', #5801 ) ;
#1755 = ORIENTED_EDGE ( 'NONE', *, *, #172, .T. ) ;
#1756 = CARTESIAN_POINT ( 'NONE',  ( 1.287237434362044075, 3.875615274277557809, -3.430618716626812059 ) ) ;
#1757 = AXIS2_PLACEMENT_3D ( 'NONE', #6982, #1032, #2515 ) ;
#1758 = ADVANCED_FACE ( 'NONE', ( #1073 ), #502, .F. ) ;
#1759 = EDGE_CURVE ( 'NONE', #3580, #1995, #8434, .T. ) ;
#1760 = CARTESIAN_POINT ( 'NONE',  ( 0.000000000000000000, 157.5000000000000284, 5.000000000000000888 ) ) ;
#1761 = CYLINDRICAL_SURFACE ( 'NONE', #7798, 10.00000000000000000 ) ;
#1762 = EDGE_CURVE ( 'NONE', #590, #7349, #1901, .T. ) ;
#1763 = LINE ( 'NONE', #5831, #5405 ) ;
#1764 = CARTESIAN_POINT ( 'NONE',  ( 136.6666666666666288, -20.00000000000000000, 162.5000000000000853 ) ) ;
#1765 = ORIENTED_EDGE ( 'NONE', *, *, #5595, .F. ) ;
#1767 = AXIS2_PLACEMENT_3D ( 'NONE', #1903, #1499, #2763 ) ;
#1766 = B_SPLINE_CURVE_WITH_KNOTS ( 'NONE', 3,
 ( #5531, #7587, #4183, #885, #217, #8203, #2233, #1669 ),
 .UNSPECIFIED., .F., .F.,
 ( 4, 2, 2, 4 ),
 ( 0.000000000000000000, 0.002450665683189820997, 0.003675998524784731495, 0.004901331366379641993 ),
 .UNSPECIFIED. ) ;
#1768 = AXIS2_PLACEMENT_3D ( 'NONE', #5592, #949, #1600 ) ;
#1769 = CARTESIAN_POINT ( 'NONE',  ( 53.33333333333330017, -20.00000000000000000, 159.8500000000001080 ) ) ;
#1770 = CARTESIAN_POINT ( 'NONE',  ( 0.000000000000000000, 0.000000000000000000, 0.000000000000000000 ) ) ;
#1771 = CARTESIAN_POINT ( 'NONE',  ( -10.00000000000000000, 1.224646799147353256E-15, -97.99999999999997158 ) ) ;
#1772 = UNCERTAINTY_MEASURE_WITH_UNIT (LENGTH_MEASURE( 1.000000000000000082E-05 ), #1714, 'distance_accuracy_value', 'NONE');
#1773 = VECTOR ( 'NONE', #4574, 1000.000000000000000 ) ;
#1774 = VECTOR ( 'NONE', #882, 1000.000000000000000 ) ;
#1775 = ORIENTED_EDGE ( 'NONE', *, *, #7658, .T. ) ;
#1776 = CARTESIAN_POINT ( 'NONE',  ( 53.33333333333330017, -20.00000000000000000, 165.1500000000000625 ) ) ;
#1777 = ORIENTED_EDGE ( 'NONE', *, *, #3453, .F. ) ;
#1778 = PRESENTATION_STYLE_ASSIGNMENT (( #7741 ) ) ;
#1779 = LINE ( 'NONE', #5156, #81 ) ;
#1780 = CONTEXT_DEPENDENT_SHAPE_REPRESENTATION ( #1973, #2744 ) ;
#1781 = VERTEX_POINT ( 'NONE', #6419 ) ;
#1782 = VERTEX_POINT ( 'NONE', #7778 ) ;
#1783 = DIRECTION ( 'NONE',  ( 1.000000000000000000, 0.000000000000000000, 0.000000000000000000 ) ) ;
#1784 = CARTESIAN_POINT ( 'NONE',  ( -5.000000000000000000, -5.000000000000000000, 148.0000000000000284 ) ) ;
#1785 = B_SPLINE_CURVE_WITH_KNOTS ( 'NONE', 3,
 ( #5837, #7858, #8512, #6301, #1902, #291 ),
 .UNSPECIFIED., .F., .F.,
 ( 4, 2, 4 ),
 ( 0.000000000000000000, 0.0002095117440854730670, 0.0004190234881709461339 ),
 .UNSPECIFIED. ) ;
#1786 = VECTOR ( 'NONE', #3275, 1000.000000000000000 ) ;
#1787 = CARTESIAN_POINT ( 'NONE',  ( 4.000000000000000888, 1.539600717838996990, -3.300726591567079815 ) ) ;
#1788 = PRODUCT_DEFINITION_SHAPE ( 'NONE', 'NONE',  #8619 ) ;
#1789 = ORIENTED_EDGE ( 'NONE', *, *, #5178, .T. ) ;
#1790 = EDGE_CURVE ( 'NONE', #5594, #3913, #1115, .T. ) ;
#1791 = DIRECTION ( 'NONE',  ( 0.000000000000000000, 0.000000000000000000, 1.000000000000000000 ) ) ;
#1792 = FACE_OUTER_BOUND ( 'NONE', #4027, .T. ) ;
#1793 = ORIENTED_EDGE ( 'NONE', *, *, #525, .T. ) ;
#1794 = ORIENTED_EDGE ( 'NONE', *, *, #2131, .F. ) ;
#1795 = DIRECTION ( 'NONE',  ( 0.000000000000000000, 0.000000000000000000, 1.000000000000000000 ) ) ;
#1796 = DIRECTION ( 'NONE',  ( 0.000000000000000000, -0.4999999999999993894, 0.8660254037844389297 ) ) ;
#1797 = DIRECTION ( 'NONE',  ( -0.000000000000000000, 1.000000000000000000, -0.000000000000000000 ) ) ;
#1798 = FACE_OUTER_BOUND ( 'NONE', #6425, .T. ) ;
#1799 = ORIENTED_EDGE ( 'NONE', *, *, #5024, .T. ) ;
#1800 = ADVANCED_FACE ( 'NONE', ( #3815 ), #4116, .T. ) ;
#1801 = ORIENTED_EDGE ( 'NONE', *, *, #2256, .F. ) ;
#1802 = DIRECTION ( 'NONE',  ( 0.000000000000000000, 0.000000000000000000, 1.000000000000000000 ) ) ;
#1803 = AXIS2_PLACEMENT_3D ( 'NONE', #4582, #6538, #8361 ) ;
#1804 = CARTESIAN_POINT ( 'NONE',  ( -0.3208286057739654917, 4.433571671609680465, -0.3503314178412548774 ) ) ;
#1805 = FACE_OUTER_BOUND ( 'NONE', #7374, .T. ) ;
#1806 = DIRECTION ( 'NONE',  ( -1.734723475976806848E-16, -1.000000000000000000, 0.000000000000000000 ) ) ;
#1807 = DIRECTION ( 'NONE',  ( 0.000000000000000000, 0.000000000000000000, 1.000000000000000000 ) ) ;
#1808 = AXIS2_PLACEMENT_3D ( 'NONE', #2841, #4317, #4797 ) ;
#1809 = ORIENTED_EDGE ( 'NONE', *, *, #8227, .T. ) ;
#1810 = EDGE_CURVE ( 'NONE', #5548, #3060, #8348, .T. ) ;
#1811 = DIRECTION ( 'NONE',  ( -0.000000000000000000, -0.000000000000000000, 1.000000000000000000 ) ) ;
#1812 = ADVANCED_FACE ( 'NONE', ( #6289 ), #7739, .F. ) ;
#1813 = LINE ( 'NONE', #3981, #1172 ) ;
#1814 = DIRECTION ( 'NONE',  ( -1.000000000000000000, 0.000000000000000000, 0.000000000000000000 ) ) ;
#1815 =( REPRESENTATION_RELATIONSHIP ('NONE','NONE', #3312, #1479 ) REPRESENTATION_RELATIONSHIP_WITH_TRANSFORMATION ( #7905 )SHAPE_REPRESENTATION_RELATIONSHIP( ) );
#1816 = VECTOR ( 'NONE', #222, 1000.000000000000000 ) ;
#1817 = ORIENTED_EDGE ( 'NONE', *, *, #3453, .T. ) ;
#1818 = DIRECTION ( 'NONE',  ( -1.000000000000000000, -0.000000000000000000, -0.000000000000000000 ) ) ;
#1819 = EDGE_LOOP ( 'NONE', ( #8004, #6667, #146, #134 ) ) ;
#1820 = PLANE ( 'NONE',  #8582 ) ;
#1821 = VECTOR ( 'NONE', #1228, 1000.000000000000000 ) ;
#1822 = ORIENTED_EDGE ( 'NONE', *, *, #1315, .F. ) ;
#1823 = VERTEX_POINT ( 'NONE', #1776 ) ;
#1824 = DIRECTION ( 'NONE',  ( -0.000000000000000000, 1.000000000000000000, -0.000000000000000000 ) ) ;
#1825 = PRODUCT_DEFINITION ( 'UNKNOWN', '', #719, #6547 ) ;
#1826 = LINE ( 'NONE', #4468, #2555 ) ;
#1827 = CARTESIAN_POINT ( 'NONE',  ( 4.211140560182196957, -2.431303136016555122, -3.745885042887436622 ) ) ;
#1828 = VERTEX_POINT ( 'NONE', #7073 ) ;
#1829 = DIRECTION ( 'NONE',  ( 6.123233995736766036E-17, -1.000000000000000000, 0.000000000000000000 ) ) ;
#1830 = DIRECTION ( 'NONE',  ( -1.734723475976806848E-16, 1.000000000000000000, 0.000000000000000000 ) ) ;
#1831 = ORIENTED_EDGE ( 'NONE', *, *, #607, .T. ) ;
#1832 = ORIENTED_EDGE ( 'NONE', *, *, #2960, .T. ) ;
#1833 = LINE ( 'NONE', #3007, #173 ) ;
#1834 = CARTESIAN_POINT ( 'NONE',  ( 2.500000000000000000, 1.178949249685218525, 2.041999999999999371 ) ) ;
#1835 = CARTESIAN_POINT ( 'NONE',  ( -5.000000000000001776, 5.000000000000001776, 140.0000000000000000 ) ) ;
#1836 = MECHANICAL_DESIGN_GEOMETRIC_PRESENTATION_REPRESENTATION (  '', ( #7674 ), #3914 ) ;
#1837 = CARTESIAN_POINT ( 'NONE',  ( -20.00000000000000000, 140.0000000000000000, 40.00000000000000000 ) ) ;
#1838 = ORIENTED_EDGE ( 'NONE', *, *, #5815, .T. ) ;
#1839 = EDGE_CURVE ( 'NONE', #702, #1160, #359, .T. ) ;
#1840 =( LENGTH_UNIT ( ) NAMED_UNIT ( * ) SI_UNIT ( .MILLI., .METRE. ) );
#1841 = VERTEX_POINT ( 'NONE', #1641 ) ;
#1842 = ORIENTED_EDGE ( 'NONE', *, *, #6954, .F. ) ;
#1843 = DIRECTION ( 'NONE',  ( -1.000000000000000000, 0.000000000000000000, -0.000000000000000000 ) ) ;
#1844 = EDGE_CURVE ( 'NONE', #7459, #1077, #3980, .T. ) ;
#1845 = AXIS2_PLACEMENT_3D ( 'NONE', #5166, #6391, #3175 ) ;
#1846 = AXIS2_PLACEMENT_3D ( 'NONE', #3961, #644, #5900 ) ;
#1847 = EDGE_CURVE ( 'NONE', #7056, #2677, #5115, .T. ) ;
#1848 = AXIS2_PLACEMENT_3D ( 'NONE', #7412, #2195, #2886 ) ;
#1849 = DIRECTION ( 'NONE',  ( -1.734723475976806848E-16, -1.000000000000000000, 0.000000000000000000 ) ) ;
#1850 = CARTESIAN_POINT ( 'NONE',  ( 0.000000000000000000, 0.000000000000000000, -4.000000000000000000 ) ) ;
#1851 = CARTESIAN_POINT ( 'NONE',  ( 5.000000000000000000, 5.000000000000000000, 148.0000000000000284 ) ) ;
#1852 = MANIFOLD_SOLID_BREP ( 'Hex', #7312 ) ;
#1853 = LINE ( 'NONE', #3485, #5109 ) ;
#1854 = AXIS2_PLACEMENT_3D ( 'NONE', #972, #2843, #2193 ) ;
#1855 = DIRECTION ( 'NONE',  ( -1.734723475976806848E-16, -1.000000000000000000, 0.000000000000000000 ) ) ;
#1856 = FACE_OUTER_BOUND ( 'NONE', #7743, .T. ) ;
#1857 = DIRECTION ( 'NONE',  ( -0.000000000000000000, -0.000000000000000000, 1.000000000000000000 ) ) ;
#1858 = AXIS2_PLACEMENT_3D ( 'NONE', #2226, #3573, #297 ) ;
#1859 = ADVANCED_FACE ( 'NONE', ( #3370 ), #2048, .T. ) ;
#1860 = AXIS2_PLACEMENT_3D ( 'NONE', #3692, #7707, #6995 ) ;
#1861 = COLOUR_RGB ( '',0.8941176470588234615, 0.8941176470588234615, 0.8941176470588234615 ) ;
#1862 = ORIENTED_EDGE ( 'NONE', *, *, #2022, .T. ) ;
#1863 = SURFACE_SIDE_STYLE ('',( #630 ) ) ;
#1864 = ADVANCED_FACE ( 'NONE', ( #4026 ), #1202, .F. ) ;
#1865 = CARTESIAN_POINT ( 'NONE',  ( -2.100000000000000089, 2.571758278209441957E-16, -5.000000000000000000 ) ) ;
#1866 = ORIENTED_EDGE ( 'NONE', *, *, #2769, .F. ) ;
#1867 =( REPRESENTATION_RELATIONSHIP ('NONE','NONE', #3312, #7993 ) REPRESENTATION_RELATIONSHIP_WITH_TRANSFORMATION ( #1554 )SHAPE_REPRESENTATION_RELATIONSHIP( ) );
#1868 = CARTESIAN_POINT ( 'NONE',  ( -5.000000000000000000, -5.000000000000000000, 140.0000000000000000 ) ) ;
#1869 = CIRCLE ( 'NONE', #6709, 2.649999999999985700 ) ;
#1870 = FACE_OUTER_BOUND ( 'NONE', #4290, .T. ) ;
#1871 = AXIS2_PLACEMENT_3D ( 'NONE', #2575, #1298, #648 ) ;
#1872 = ADVANCED_FACE ( 'NONE', ( #3858 ), #3286, .F. ) ;
#1873 = CARTESIAN_POINT ( 'NONE',  ( -4.000000000000000000, -1.560351142792950618, -0.2242961665059814425 ) ) ;
#1874 = VERTEX_POINT ( 'NONE', #4583 ) ;
#1875 = DIRECTION ( 'NONE',  ( -1.000000000000000000, 0.000000000000000000, 0.000000000000000000 ) ) ;
#1876 = CIRCLE ( 'NONE', #608, 10.00000000000000000 ) ;
#1877 = DIRECTION ( 'NONE',  ( -0.000000000000000000, -0.000000000000000000, -1.000000000000000000 ) ) ;
#1878 = VERTEX_POINT ( 'NONE', #541 ) ;
#1879 = EDGE_LOOP ( 'NONE', ( #4286, #2247, #979, #604 ) ) ;
#1880 = DIRECTION ( 'NONE',  ( -0.000000000000000000, -0.000000000000000000, 1.000000000000000000 ) ) ;
#1881 = CARTESIAN_POINT ( 'NONE',  ( -4.999999999999998224, -4.999999999999998224, 139.9990000000000236 ) ) ;
#1882 = VECTOR ( 'NONE', #5565, 1000.000000000000114 ) ;
#1883 = DIRECTION ( 'NONE',  ( 1.000000000000000000, 1.734723475976807587E-16, 0.000000000000000000 ) ) ;
#1884 = DIRECTION ( 'NONE',  ( 0.000000000000000000, 1.000000000000000000, 0.000000000000000000 ) ) ;
#1885 = ORIENTED_EDGE ( 'NONE', *, *, #794, .T. ) ;
#1886 = SURFACE_SIDE_STYLE ('',( #1099 ) ) ;
#1887 = ORIENTED_EDGE ( 'NONE', *, *, #3719, .F. ) ;
#1888 = CARTESIAN_POINT ( 'NONE',  ( 2.500000000000000000, 2.357898499370433054, -1.951563910473907981E-15 ) ) ;
#1889 = EDGE_CURVE ( 'NONE', #3427, #4515, #5927, .T. ) ;
#1890 = FACE_OUTER_BOUND ( 'NONE', #7744, .T. ) ;
#1891 = DIRECTION ( 'NONE',  ( -1.000000000000000000, 0.000000000000000000, 0.000000000000000000 ) ) ;
#1892 = EDGE_CURVE ( 'NONE', #7220, #7011, #1236, .T. ) ;
#1893 = LINE ( 'NONE', #7103, #7080 ) ;
#1894 = DIRECTION ( 'NONE',  ( 0.000000000000000000, 0.000000000000000000, 1.000000000000000000 ) ) ;
#1895 = EDGE_CURVE ( 'NONE', #2697, #6761, #3946, .T. ) ;
#1896 = DIRECTION ( 'NONE',  ( 1.734723475976807587E-16, 1.000000000000000000, 0.000000000000000000 ) ) ;
#1897 = AXIS2_PLACEMENT_3D ( 'NONE', #380, #4995, #2998 ) ;
#1898 = CARTESIAN_POINT ( 'NONE',  ( -5.000000000000001776, 5.000000000000001776, -143.0000000000000284 ) ) ;
#1899 = LINE ( 'NONE', #3456, #7260 ) ;
#1900 = ADVANCED_BREP_SHAPE_REPRESENTATION ( '', ( #4686, #594 ), #1694 ) ;
#1901 = CIRCLE ( 'NONE', #4663, 2.649999999999985700 ) ;
#1902 = CARTESIAN_POINT ( 'NONE',  ( 4.154306624731137099, 2.398490048084935822, -3.721999068284414847 ) ) ;
#1903 = CARTESIAN_POINT ( 'NONE',  ( 439.9999999999999432, -25.00000000000000000, 18.96857495968446017 ) ) ;
#1904 = CIRCLE ( 'NONE', #2038, 2.649999999999985700 ) ;
#1905 = VERTEX_POINT ( 'NONE', #4541 ) ;
#1906 = FACE_BOUND ( 'NONE', #8099, .T. ) ;
#1907 = VERTEX_POINT ( 'NONE', #6666 ) ;
#1908 = CARTESIAN_POINT ( 'NONE',  ( 1.567478505476134606E-15, 4.618802153517012066, -3.433295621305382905 ) ) ;
#1909 = CARTESIAN_POINT ( 'NONE',  ( 352.0000000000000000, -20.00000000000000000, -18.88142504031545243 ) ) ;
#1910 = VECTOR ( 'NONE', #4669, 1000.000000000000000 ) ;
#1911 = VECTOR ( 'NONE', #2188, 1000.000000000000000 ) ;
#1912 = LINE ( 'NONE', #4549, #3150 ) ;
#1913 = ORIENTED_EDGE ( 'NONE', *, *, #4759, .T. ) ;
#1914 = CARTESIAN_POINT ( 'NONE',  ( 5.000000000000000000, -5.000000000000000000, 140.0000000000000000 ) ) ;
#1915 = CARTESIAN_POINT ( 'NONE',  ( -3.061616997868376239E-16, -10.00000000000000178, -157.5000000000000284 ) ) ;
#1916 = CARTESIAN_POINT ( 'NONE',  ( 5.000000000000000000, -5.000000000000000000, 140.0000000000000000 ) ) ;
#1917 = VERTEX_POINT ( 'NONE', #8513 ) ;
#1918 = ORIENTED_EDGE ( 'NONE', *, *, #3084, .F. ) ;
#1919 = EDGE_CURVE ( 'NONE', #7049, #3079, #3246, .T. ) ;
#1920 = CARTESIAN_POINT ( 'NONE',  ( 2.500000000000000000, 2.357898499370433054, -1.951563910473907981E-15 ) ) ;
#1921 = B_SPLINE_CURVE_WITH_KNOTS ( 'NONE', 3,
 ( #7787, #2356, #1082, #7661, #423, #1827 ),
 .UNSPECIFIED., .F., .F.,
 ( 4, 2, 4 ),
 ( 0.002452478801916361129, 0.003676905084148001344, 0.004901331366379641126 ),
 .UNSPECIFIED. ) ;
#1922 = EDGE_CURVE ( 'NONE', #2428, #1985, #5503, .T. ) ;
#1923 = CARTESIAN_POINT ( 'NONE',  ( -4.000000000000000000, -2.309401076758512694, -5.000000000000000000 ) ) ;
#1924 = VECTOR ( 'NONE', #618, 1000.000000000000000 ) ;
#1925 = FACE_OUTER_BOUND ( 'NONE', #4951, .T. ) ;
#1926 = PLANE ( 'NONE',  #5252 ) ;
#1927 = ORIENTED_EDGE ( 'NONE', *, *, #4704, .F. ) ;
#1928 = VECTOR ( 'NONE', #40, 1000.000000000000000 ) ;
#1929 = EDGE_LOOP ( 'NONE', ( #6294, #2936, #2091, #3597 ) ) ;
#1930 = DIRECTION ( 'NONE',  ( 0.000000000000000000, 0.000000000000000000, 1.000000000000000000 ) ) ;
#1931 = EDGE_CURVE ( 'NONE', #2500, #5031, #8160, .T. ) ;
#1932 = DIRECTION ( 'NONE',  ( 1.000000000000000000, 0.000000000000000000, 0.000000000000000000 ) ) ;
#1933 = DIRECTION ( 'NONE',  ( -1.000000000000000000, 0.000000000000000000, -0.000000000000000000 ) ) ;
#1934 = DIRECTION ( 'NONE',  ( 0.000000000000000000, 0.000000000000000000, 1.000000000000000000 ) ) ;
#1935 = LINE ( 'NONE', #6496, #3584 ) ;
#1936 = VECTOR ( 'NONE', #6086, 1000.000000000000114 ) ;
#1937 = CARTESIAN_POINT ( 'NONE',  ( 82.99999999999998579, -4.999999999999998224, 145.0000000000000284 ) ) ;
#1938 = CARTESIAN_POINT ( 'NONE',  ( 5.000000000000000000, -5.000000000000000000, 148.0000000000000284 ) ) ;
#1939 = DIRECTION ( 'NONE',  ( -0.000000000000000000, -1.000000000000000000, -0.000000000000000000 ) ) ;
#1940 = CIRCLE ( 'NONE', #2504, 2.649999999999985700 ) ;
#1941 = DIRECTION ( 'NONE',  ( -1.000000000000000000, 0.000000000000000000, 0.000000000000000000 ) ) ;
#1942 = DIRECTION ( 'NONE',  ( -0.000000000000000000, 1.000000000000000000, -0.000000000000000000 ) ) ;
#1943 = PRESENTATION_STYLE_ASSIGNMENT (( #7901 ) ) ;
#1944 = ORIENTED_EDGE ( 'NONE', *, *, #3170, .F. ) ;
#1945 = CARTESIAN_POINT ( 'NONE',  ( -4.000000000000000000, 0.000000000000000000, 0.000000000000000000 ) ) ;
#1946 = ORIENTED_EDGE ( 'NONE', *, *, #5666, .T. ) ;
#1947 = CYLINDRICAL_SURFACE ( 'NONE', #6109, 2.649999999999985700 ) ;
#1948 = AXIS2_PLACEMENT_3D ( 'NONE', #1229, #8426, #1722 ) ;
#1949 = EDGE_CURVE ( 'NONE', #24, #2756, #1363, .T. ) ;
#1950 = LINE ( 'NONE', #6510, #740 ) ;
#1951 = PRODUCT_DEFINITION_CONTEXT ( 'detailed design', #472, 'design' ) ;
#1952 = EDGE_CURVE ( 'NONE', #4515, #7275, #5197, .T. ) ;
#1953 = FACE_OUTER_BOUND ( 'NONE', #5385, .T. ) ;
#1954 = AXIS2_PLACEMENT_3D ( 'NONE', #5830, #3022, #4451 ) ;
#1955 = ORIENTED_EDGE ( 'NONE', *, *, #976, .F. ) ;
#1956 = CARTESIAN_POINT ( 'NONE',  ( 4.197393957002303999, 7.772902908466098641E-14, -3.503767560748929810 ) ) ;
#1957 = DIRECTION ( 'NONE',  ( 0.6000000000000011990, 5.551115123125782702E-17, 0.7999999999999990452 ) ) ;
#1958 = CARTESIAN_POINT ( 'NONE',  ( -20.00000000000000000, 175.0000000000000284, 5.000000000000000000 ) ) ;
#1959 = VERTEX_POINT ( 'NONE', #7859 ) ;
#1960 = ORIENTED_EDGE ( 'NONE', *, *, #8465, .F. ) ;
#1961 = CARTESIAN_POINT ( 'NONE',  ( -30.00000000000002842, -20.00000000000000000, -200.0000000000000000 ) ) ;
#1962 = DIRECTION ( 'NONE',  ( -1.000000000000000000, 0.000000000000000000, 0.000000000000000000 ) ) ;
#1963 = CARTESIAN_POINT ( 'NONE',  ( 4.211399257449709665, -2.459727064652517114, -3.751161691472417736 ) ) ;
#1964 = EDGE_CURVE ( 'NONE', #3298, #4682, #3897, .T. ) ;
#1965 = DIRECTION ( 'NONE',  ( -0.000000000000000000, 1.000000000000000000, -0.000000000000000000 ) ) ;
#1966 = ORIENTED_EDGE ( 'NONE', *, *, #6635, .F. ) ;
#1967 = VERTEX_POINT ( 'NONE', #7197 ) ;
#1968 = CARTESIAN_POINT ( 'NONE',  ( -4.999999999999998224, 134.9989999999999952, 25.00000000000000000 ) ) ;
#1969 = DIRECTION ( 'NONE',  ( -1.000000000000000000, 0.000000000000000000, 0.000000000000000000 ) ) ;
#1970 = CARTESIAN_POINT ( 'NONE',  ( 25.00000000000000000, 2.789133085058098087E-16, -2.055000000000000160 ) ) ;
#1971 = ORIENTED_EDGE ( 'NONE', *, *, #2809, .T. ) ;
#1972 = CARTESIAN_POINT ( 'NONE',  ( 20.00000000000000000, 0.000000000000000000, -154.5685424949238040 ) ) ;
#1973 =( REPRESENTATION_RELATIONSHIP ('NONE','NONE', #3312, #4754 ) REPRESENTATION_RELATIONSHIP_WITH_TRANSFORMATION ( #6070 )SHAPE_REPRESENTATION_RELATIONSHIP( ) );
#1974 = PRODUCT_RELATED_PRODUCT_CATEGORY ( 'part', '', ( #3920 ) ) ;
#1975 = DIRECTION ( 'NONE',  ( 0.000000000000000000, 0.000000000000000000, 1.000000000000000000 ) ) ;
#1976 = AXIS2_PLACEMENT_3D ( 'NONE', #2550, #536, #7773 ) ;
#1977 = CARTESIAN_POINT ( 'NONE',  ( 0.000000000000000000, 0.000000000000000000, 120.0000000000000142 ) ) ;
#1978 = DIRECTION ( 'NONE',  ( 0.000000000000000000, 0.000000000000000000, 1.000000000000000000 ) ) ;
#1979 = DIRECTION ( 'NONE',  ( -0.000000000000000000, -0.000000000000000000, 1.000000000000000000 ) ) ;
#1980 = VECTOR ( 'NONE', #86, 1000.000000000000000 ) ;
#1981 = LINE ( 'NONE', #6757, #3605 ) ;
#1982 = DIRECTION ( 'NONE',  ( 0.000000000000000000, 0.000000000000000000, 1.000000000000000000 ) ) ;
#1983 = ORIENTED_EDGE ( 'NONE', *, *, #5161, .T. ) ;
#1984 = ORIENTED_EDGE ( 'NONE', *, *, #6886, .F. ) ;
#1985 = VERTEX_POINT ( 'NONE', #1321 ) ;
#1986 = MANIFOLD_SOLID_BREP ( 'Boss-Extrude4', #1329 ) ;
#1987 = AXIS2_PLACEMENT_3D ( 'NONE', #5470, #3435, #4736 ) ;
#1988 = DIRECTION ( 'NONE',  ( -1.000000000000000000, 1.734723475976807341E-16, -0.000000000000000000 ) ) ;
#1989 = AXIS2_PLACEMENT_3D ( 'NONE', #5997, #3404, #5221 ) ;
#1990 = DIRECTION ( 'NONE',  ( 0.000000000000000000, 0.000000000000000000, 1.000000000000000000 ) ) ;
#1991 = CIRCLE ( 'NONE', #735, 2.100000000000000089 ) ;
#1992 = EDGE_CURVE ( 'NONE', #2774, #8517, #6758, .T. ) ;
#1993 = DIRECTION ( 'NONE',  ( 0.000000000000000000, 0.4999999999999993894, -0.8660254037844389297 ) ) ;
#1994 = EDGE_CURVE ( 'NONE', #2349, #6072, #80, .T. ) ;
#1995 = VERTEX_POINT ( 'NONE', #4189 ) ;
#1996 = CIRCLE ( 'NONE', #3523, 20.00000000000000000 ) ;
#1997 = DIRECTION ( 'NONE',  ( 0.000000000000000000, -1.000000000000000000, 0.000000000000000000 ) ) ;
#1998 = FACE_BOUND ( 'NONE', #4292, .T. ) ;
#1999 = DIRECTION ( 'NONE',  ( -1.040834085586084257E-17, -0.9999999999999998890, -5.551115123125782702E-17 ) ) ;
#2000 = LINE ( 'NONE', #3910, #8403 ) ;
#2001 = ORIENTED_EDGE ( 'NONE', *, *, #2128, .T. ) ;
#2002 = EDGE_CURVE ( 'NONE', #2677, #3177, #3589, .T. ) ;
#2003 = VECTOR ( 'NONE', #5726, 1000.000000000000000 ) ;
#2004 = EDGE_LOOP ( 'NONE', ( #4240, #6741, #4572, #4137 ) ) ;
#2005 =( GEOMETRIC_REPRESENTATION_CONTEXT ( 3 ) GLOBAL_UNCERTAINTY_ASSIGNED_CONTEXT ( ( #3765 ) ) GLOBAL_UNIT_ASSIGNED_CONTEXT ( ( #3146, #8499, #3795 ) ) REPRESENTATION_CONTEXT ( 'NONE', 'WORKASPACE' ) );
#2006 = CARTESIAN_POINT ( 'NONE',  ( 259.0000000000000000, -4.999999999999998224, 140.0000000000000000 ) ) ;
#2007 = PLANE ( 'NONE',  #4640 ) ;
#2008 = CIRCLE ( 'NONE', #6858, 10.00000000000000000 ) ;
#2009 = AXIS2_PLACEMENT_3D ( 'NONE', #717, #3029, #3115 ) ;
#2010 = CARTESIAN_POINT ( 'NONE',  ( 4.000000000000000000, 2.512223110932545023, -3.469391141908803711 ) ) ;
#2011 = DIRECTION ( 'NONE',  ( 0.000000000000000000, 0.000000000000000000, 1.000000000000000000 ) ) ;
#2012 = ORIENTED_EDGE ( 'NONE', *, *, #5741, .F. ) ;
#2013 = EDGE_LOOP ( 'NONE', ( #7119, #1866 ) ) ;
#2014 = FACE_OUTER_BOUND ( 'NONE', #2995, .T. ) ;
#2015 = VECTOR ( 'NONE', #5613, 999.9999999999998863 ) ;
#2016 = CYLINDRICAL_SURFACE ( 'NONE', #1344, 2.649999999999985700 ) ;
#2017 = PLANE ( 'NONE',  #2348 ) ;
#2018 = ORIENTED_EDGE ( 'NONE', *, *, #4563, .F. ) ;
#2019 = PLANE ( 'NONE',  #1530 ) ;
#2020 = CARTESIAN_POINT ( 'NONE',  ( 0.000000000000000000, 0.000000000000000000, -27.99999999999999645 ) ) ;
#2021 = FACE_BOUND ( 'NONE', #952, .T. ) ;
#2022 = EDGE_CURVE ( 'NONE', #1026, #7552, #105, .T. ) ;
#2023 = EDGE_CURVE ( 'NONE', #678, #807, #6612, .T. ) ;
#2024 = CARTESIAN_POINT ( 'NONE',  ( 4.000000000000003553, -2.309401076758513138, -3.504271511726786859 ) ) ;
#2025 = EDGE_CURVE ( 'NONE', #4249, #2756, #8082, .T. ) ;
#2026 = DIRECTION ( 'NONE',  ( 0.000000000000000000, 0.000000000000000000, -1.000000000000000000 ) ) ;
#2027 = DIRECTION ( 'NONE',  ( 0.000000000000000000, 0.000000000000000000, 1.000000000000000000 ) ) ;
#2028 =( LENGTH_UNIT ( ) NAMED_UNIT ( * ) SI_UNIT ( .MILLI., .METRE. ) );
#2029 = EDGE_LOOP ( 'NONE', ( #7948, #4445, #4555, #5, #8067 ) ) ;
#2030 =( LENGTH_UNIT ( ) NAMED_UNIT ( * ) SI_UNIT ( .MILLI., .METRE. ) );
#2031 = AXIS2_PLACEMENT_3D ( 'NONE', #7843, #4482, #3058 ) ;
#2032 = ORIENTED_EDGE ( 'NONE', *, *, #6244, .F. ) ;
#2033 = ORIENTED_EDGE ( 'NONE', *, *, #3534, .F. ) ;
#2034 = DIRECTION ( 'NONE',  ( -0.000000000000000000, 1.000000000000000000, -0.000000000000000000 ) ) ;
#2035 = DIRECTION ( 'NONE',  ( -0.000000000000000000, 1.000000000000000000, -0.000000000000000000 ) ) ;
#2036 = ADVANCED_FACE ( 'NONE', ( #93 ), #2889, .T. ) ;
#2037 = VECTOR ( 'NONE', #5205, 1000.000000000000000 ) ;
#2038 = AXIS2_PLACEMENT_3D ( 'NONE', #4251, #6901, #4860 ) ;
#2039 = EDGE_LOOP ( 'NONE', ( #1597, #2190 ) ) ;
#2040 = DIRECTION ( 'NONE',  ( 0.000000000000000000, 0.4999999999999993339, -0.8660254037844390407 ) ) ;
#2041 = EDGE_LOOP ( 'NONE', ( #4308, #5411, #1252, #4808, #5569 ) ) ;
#2042 = DIRECTION ( 'NONE',  ( 1.000000000000000000, 0.000000000000000000, 0.000000000000000000 ) ) ;
#2043 = CARTESIAN_POINT ( 'NONE',  ( 2.500000000000000000, 0.000000000000000000, 0.000000000000000000 ) ) ;
#2044 = CARTESIAN_POINT ( 'NONE',  ( 352.0000000000000000, -30.00000000000002842, -16.23142504031548228 ) ) ;
#2045 = DIRECTION ( 'NONE',  ( 0.000000000000000000, 0.000000000000000000, -1.000000000000000000 ) ) ;
#2046 = ORIENTED_EDGE ( 'NONE', *, *, #5828, .T. ) ;
#2047 = ORIENTED_EDGE ( 'NONE', *, *, #7067, .F. ) ;
#2048 = CONICAL_SURFACE ( 'NONE', #8307, 2.055000000000000160, 0.7853981633974721488 ) ;
#2050 = AXIS2_PLACEMENT_3D ( 'NONE', #1444, #5307, #4794 ) ;
#2049 = CARTESIAN_POINT ( 'NONE',  ( 0.000000000000000000, 0.000000000000000000, -97.99999999999997158 ) ) ;
#2051 = LINE ( 'NONE', #1923, #4371 ) ;
#2052 = EDGE_CURVE ( 'NONE', #6060, #884, #1627, .T. ) ;
#2053 = CARTESIAN_POINT ( 'NONE',  ( 4.000000000000000000, 1.680228229147133767, -3.316631783032546021 ) ) ;
#2054 = VECTOR ( 'NONE', #7575, 1000.000000000000000 ) ;
#2055 = CARTESIAN_POINT ( 'NONE',  ( 181.0000000000000000, 5.000000000000000000, 140.0000000000000000 ) ) ;
#2056 = VERTEX_POINT ( 'NONE', #7457 ) ;
#2057 =( NAMED_UNIT ( * ) PLANE_ANGLE_UNIT ( ) SI_UNIT ( $, .RADIAN. ) );
#2058 = EDGE_LOOP ( 'NONE', ( #5168, #7419, #5067, #3478 ) ) ;
#2059 = DIRECTION ( 'NONE',  ( 0.000000000000000000, 0.000000000000000000, 1.000000000000000000 ) ) ;
#2060 = EDGE_CURVE ( 'NONE', #2610, #7663, #5783, .T. ) ;
#2061 = ADVANCED_FACE ( 'NONE', ( #6711, #764 ), #6849, .T. ) ;
#2062 = CARTESIAN_POINT ( 'NONE',  ( 5.000000000000000000, -5.000000000000000000, 148.0000000000000284 ) ) ;
#2063 = CARTESIAN_POINT ( 'NONE',  ( 5.000000000000000000, -5.000000000000000000, 148.0000000000000284 ) ) ;
#2064 = ORIENTED_EDGE ( 'NONE', *, *, #7333, .F. ) ;
#2065 = CYLINDRICAL_SURFACE ( 'NONE', #835, 2.649999999999985700 ) ;
#2066 = PLANE ( 'NONE',  #4065 ) ;
#2067 = CARTESIAN_POINT ( 'NONE',  ( -5.000000000000001776, 5.000000000000001776, 34.00000000000000711 ) ) ;
#2068 = CARTESIAN_POINT ( 'NONE',  ( 0.000000000000000000, 0.000000000000000000, -97.99999999999997158 ) ) ;
#2069 = DIRECTION ( 'NONE',  ( 0.000000000000000000, 1.000000000000000000, 0.000000000000000000 ) ) ;
#2070 = EDGE_CURVE ( 'NONE', #4673, #4209, #5090, .T. ) ;
#2071 = VECTOR ( 'NONE', #4881, 1000.000000000000000 ) ;
#2072 = ORIENTED_EDGE ( 'NONE', *, *, #2603, .T. ) ;
#2073 = EDGE_LOOP ( 'NONE', ( #4749, #5157, #4998, #4326 ) ) ;
#2074 = UNCERTAINTY_MEASURE_WITH_UNIT (LENGTH_MEASURE( 1.000000000000000082E-05 ), #6421, 'distance_accuracy_value', 'NONE');
#2075 = ORIENTED_EDGE ( 'NONE', *, *, #1348, .T. ) ;
#2076 = DIRECTION ( 'NONE',  ( 0.000000000000000000, 0.000000000000000000, 1.000000000000000000 ) ) ;
#2077 = DIRECTION ( 'NONE',  ( -1.000000000000000000, 1.734723475976807587E-16, 0.000000000000000000 ) ) ;
#2078 = ORIENTED_EDGE ( 'NONE', *, *, #3296, .T. ) ;
#2079 = DIRECTION ( 'NONE',  ( -1.000000000000000000, 0.000000000000000000, -0.000000000000000000 ) ) ;
#2080 = VERTEX_POINT ( 'NONE', #846 ) ;
#2081 = DIRECTION ( 'NONE',  ( 1.000000000000000000, 0.000000000000000000, 0.000000000000000000 ) ) ;
#2082 = CARTESIAN_POINT ( 'NONE',  ( -20.00000000000000000, 140.0000000000000000, 0.000000000000000000 ) ) ;
#2083 = VECTOR ( 'NONE', #839, 1000.000000000000000 ) ;
#2084 = ORIENTED_EDGE ( 'NONE', *, *, #5522, .F. ) ;
#2085 = ORIENTED_EDGE ( 'NONE', *, *, #6319, .T. ) ;
#2086 = LINE ( 'NONE', #4166, #8523 ) ;
#2087 = DIRECTION ( 'NONE',  ( -1.000000000000000000, 0.000000000000000000, 0.000000000000000000 ) ) ;
#2088 = VECTOR ( 'NONE', #1675, 1000.000000000000000 ) ;
#2089 = CARTESIAN_POINT ( 'NONE',  ( 170.9999999999999716, -4.999999999999998224, 145.0000000000000284 ) ) ;
#2090 = LINE ( 'NONE', #2593, #5948 ) ;
#2091 = ORIENTED_EDGE ( 'NONE', *, *, #7723, .F. ) ;
#2092 = FACE_OUTER_BOUND ( 'NONE', #2401, .T. ) ;
#2093 = ORIENTED_EDGE ( 'NONE', *, *, #6636, .F. ) ;
#2094 = ORIENTED_EDGE ( 'NONE', *, *, #4865, .T. ) ;
#2095 = PLANE ( 'NONE',  #8120 ) ;
#2096 = LINE ( 'NONE', #4614, #4128 ) ;
#2097 = EDGE_CURVE ( 'NONE', #392, #8131, #8166, .T. ) ;
#2098 = CARTESIAN_POINT ( 'NONE',  ( -5.000000000000001776, 5.000000000000001776, 148.0000000000000284 ) ) ;
#2099 = ORIENTED_EDGE ( 'NONE', *, *, #7670, .T. ) ;
#2100 = CARTESIAN_POINT ( 'NONE',  ( -4.211140560182196957, 2.431303136016537803, -3.745885042887433514 ) ) ;
#2101 = ADVANCED_FACE ( 'NONE', ( #6145 ), #3501, .T. ) ;
#2102 = DIRECTION ( 'NONE',  ( -0.000000000000000000, 1.000000000000000000, -0.000000000000000000 ) ) ;
#2103 = EDGE_CURVE ( 'NONE', #1013, #5774, #2240, .T. ) ;
#2104 = DIRECTION ( 'NONE',  ( 0.000000000000000000, 0.000000000000000000, -1.000000000000000000 ) ) ;
#2105 = DIRECTION ( 'NONE',  ( 0.000000000000000000, 0.000000000000000000, -1.000000000000000000 ) ) ;
#2106 = DIRECTION ( 'NONE',  ( 0.000000000000000000, 0.000000000000000000, -1.000000000000000000 ) ) ;
#2107 = ORIENTED_EDGE ( 'NONE', *, *, #7155, .T. ) ;
#2108 = ORIENTED_EDGE ( 'NONE', *, *, #2127, .T. ) ;
#2109 = ORIENTED_EDGE ( 'NONE', *, *, #5103, .F. ) ;
#2110 = CARTESIAN_POINT ( 'NONE',  ( 219.9999999999999716, -14.99999999999999822, 162.5000000000000853 ) ) ;
#2111 = CARTESIAN_POINT ( 'NONE',  ( 176.0000000000000000, -25.00000000000000000, -89.28142504031545457 ) ) ;
#2112 = EDGE_CURVE ( 'NONE', #7579, #6119, #5229, .T. ) ;
#2113 = AXIS2_PLACEMENT_3D ( 'NONE', #7653, #5071, #1733 ) ;
#2114 = VECTOR ( 'NONE', #6534, 1000.000000000000000 ) ;
#2115 = ORIENTED_EDGE ( 'NONE', *, *, #6954, .T. ) ;
#2116 = PLANE ( 'NONE',  #8301 ) ;
#2117 = VECTOR ( 'NONE', #5392, 1000.000000000000000 ) ;
#2118 = EDGE_LOOP ( 'NONE', ( #319, #2269 ) ) ;
#2119 = CARTESIAN_POINT ( 'NONE',  ( 53.33333333333330017, -20.00000000000000000, 165.1500000000000625 ) ) ;
#2120 = CARTESIAN_POINT ( 'NONE',  ( 0.000000000000000000, 0.000000000000000000, 120.0000000000000284 ) ) ;
#2121 = ORIENTED_EDGE ( 'NONE', *, *, #1992, .F. ) ;
#2122 = AXIS2_PLACEMENT_3D ( 'NONE', #4845, #1537, #4184 ) ;
#2123 = ORIENTED_EDGE ( 'NONE', *, *, #7795, .F. ) ;
#2124 = CARTESIAN_POINT ( 'NONE',  ( 386.6666666666666288, -25.00000000000000000, 162.5000000000000853 ) ) ;
#2125 = DIRECTION ( 'NONE',  ( -1.000000000000000000, 1.734723475976807587E-16, 0.000000000000000000 ) ) ;
#2126 = VECTOR ( 'NONE', #1567, 1000.000000000000000 ) ;
#2127 = EDGE_CURVE ( 'NONE', #3415, #5774, #4453, .T. ) ;
#2128 = EDGE_CURVE ( 'NONE', #5009, #3592, #3111, .T. ) ;
#2129 = MANIFOLD_SOLID_BREP ( 'M5 Clearance Hole1', #3987 ) ;
#2130 = CIRCLE ( 'NONE', #2421, 10.00000000000000000 ) ;
#2131 = EDGE_CURVE ( 'NONE', #7651, #7275, #7730, .T. ) ;
#2132 = DIRECTION ( 'NONE',  ( 1.000000000000000000, 0.000000000000000000, 0.000000000000000000 ) ) ;
#2133 = FACE_OUTER_BOUND ( 'NONE', #5563, .T. ) ;
#2134 = EDGE_LOOP ( 'NONE', ( #6237, #1088 ) ) ;
#2135 = CARTESIAN_POINT ( 'NONE',  ( -5.000000000000000000, -5.000000000000000000, -63.99999999999997158 ) ) ;
#2136 = PRESENTATION_LAYER_ASSIGNMENT (  '', '', ( #33 ) ) ;
#2137 = COLOUR_RGB ( '',0.8941176470588234615, 0.8941176470588234615, 0.8941176470588234615 ) ;
#2138 = DIRECTION ( 'NONE',  ( 1.000000000000000000, 0.000000000000000000, 0.000000000000000000 ) ) ;
#2139 = CARTESIAN_POINT ( 'NONE',  ( 0.000000000000000000, 0.000000000000000000, 7.000000000000006217 ) ) ;
#2140 = EDGE_LOOP ( 'NONE', ( #2982, #4100, #4359, #5653 ) ) ;
#2141 = ORIENTED_EDGE ( 'NONE', *, *, #6559, .F. ) ;
#2142 = CARTESIAN_POINT ( 'NONE',  ( -2.000000000000006661, 3.464101615137750834, 0.000000000000000000 ) ) ;
#2143 =( REPRESENTATION_RELATIONSHIP ('NONE','NONE', #3312, #872 ) REPRESENTATION_RELATIONSHIP_WITH_TRANSFORMATION ( #7118 )SHAPE_REPRESENTATION_RELATIONSHIP( ) );
#2144 = AXIS2_PLACEMENT_3D ( 'NONE', #2768, #3419, #6854 ) ;
#2145 = DIRECTION ( 'NONE',  ( -1.000000000000000000, 0.000000000000000000, 0.000000000000000000 ) ) ;
#2146 = CYLINDRICAL_SURFACE ( 'NONE', #1096, 10.00000000000000000 ) ;
#2147 = EDGE_LOOP ( 'NONE', ( #4820, #3136, #8, #6022 ) ) ;
#2148 = DIRECTION ( 'NONE',  ( -0.000000000000000000, 1.000000000000000000, -0.000000000000000000 ) ) ;
#2149 = EDGE_CURVE ( 'NONE', #7520, #8365, #7323, .T. ) ;
#2150 = DIRECTION ( 'NONE',  ( -1.000000000000000000, 0.000000000000000000, 0.000000000000000000 ) ) ;
#2151 = FACE_OUTER_BOUND ( 'NONE', #818, .T. ) ;
#2152 = DIRECTION ( 'NONE',  ( 1.000000000000000000, 0.000000000000000000, 0.000000000000000000 ) ) ;
#2153 = ADVANCED_FACE ( 'NONE', ( #7062 ), #4269, .T. ) ;
#2154 = DIRECTION ( 'NONE',  ( 1.734723475976806848E-16, -1.000000000000000000, -0.000000000000000000 ) ) ;
#2155 = CARTESIAN_POINT ( 'NONE',  ( 4.000000000000000000, -1.942223658245635809, -0.3516579909967643691 ) ) ;
#2156 = ORIENTED_EDGE ( 'NONE', *, *, #6669, .T. ) ;
#2157 = EDGE_LOOP ( 'NONE', ( #4864, #7382 ) ) ;
#2158 = EDGE_LOOP ( 'NONE', ( #7240, #5370, #4894, #5430 ) ) ;
#2159 = DIRECTION ( 'NONE',  ( 0.000000000000000000, 0.000000000000000000, -1.000000000000000000 ) ) ;
#2160 = PLANE ( 'NONE',  #7138 ) ;
#2161 = ORIENTED_EDGE ( 'NONE', *, *, #3865, .T. ) ;
#2162 = CARTESIAN_POINT ( 'NONE',  ( 259.0000000000000000, -4.999999999999998224, 139.9990000000000236 ) ) ;
#2163 = ORIENTED_EDGE ( 'NONE', *, *, #7799, .F. ) ;
#2164 = CARTESIAN_POINT ( 'NONE',  ( 3.511755186886750923, -2.826662030176382956, -3.597382984111582083 ) ) ;
#2165 = CARTESIAN_POINT ( 'NONE',  ( 0.000000000000000000, 0.000000000000000000, 0.000000000000000000 ) ) ;
#2166 = SURFACE_STYLE_FILL_AREA ( #8053 ) ;
#2167 = EDGE_LOOP ( 'NONE', ( #5720, #6981, #4273, #2232 ) ) ;
#2168 = EDGE_LOOP ( 'NONE', ( #8562, #5106, #3391, #4728 ) ) ;
#2169 = DIRECTION ( 'NONE',  ( -1.000000000000000000, -0.000000000000000000, -0.000000000000000000 ) ) ;
#2170 = CARTESIAN_POINT ( 'NONE',  ( 0.000000000000000000, 2.357898499370433054, -1.951563910473907981E-15 ) ) ;
#2171 = AXIS2_PLACEMENT_3D ( 'NONE', #3309, #5215, #1303 ) ;
#2172 = DIRECTION ( 'NONE',  ( 1.000000000000000000, 0.000000000000000000, 0.000000000000000000 ) ) ;
#2173 = CARTESIAN_POINT ( 'NONE',  ( -2.649999999999993694, 157.5000000000000284, 5.000000000000000000 ) ) ;
#2174 = VERTEX_POINT ( 'NONE', #5105 ) ;
#2175 = DIRECTION ( 'NONE',  ( 1.000000000000000000, 0.000000000000000000, 0.000000000000000000 ) ) ;
#2176 = VECTOR ( 'NONE', #1158, 1000.000000000000000 ) ;
#2177 = EDGE_CURVE ( 'NONE', #2249, #1907, #8031, .T. ) ;
#2178 = CIRCLE ( 'NONE', #220, 2.649999999999985700 ) ;
#2179 =( LENGTH_UNIT ( ) NAMED_UNIT ( * ) SI_UNIT ( .MILLI., .METRE. ) );
#2180 = LINE ( 'NONE', #2788, #7543 ) ;
#2181 = VERTEX_POINT ( 'NONE', #1632 ) ;
#2182 = EDGE_CURVE ( 'NONE', #5694, #3602, #5625, .T. ) ;
#2183 = EDGE_LOOP ( 'NONE', ( #2863, #2072 ) ) ;
#2184 = CARTESIAN_POINT ( 'NONE',  ( -0.5469614295416921346, 4.303013824936271270, -3.535263753543735454 ) ) ;
#2185 = LINE ( 'NONE', #5526, #2015 ) ;
#2186 = COLOUR_RGB ( '',0.8941176470588234615, 0.8941176470588234615, 0.8941176470588234615 ) ;
#2187 = CIRCLE ( 'NONE', #6212, 10.00000000000000000 ) ;
#2188 = DIRECTION ( 'NONE',  ( -1.734723475976807341E-16, 1.000000000000000000, 0.000000000000000000 ) ) ;
#2189 = DIRECTION ( 'NONE',  ( 0.000000000000000000, 1.000000000000000000, 0.000000000000000000 ) ) ;
#2190 = ORIENTED_EDGE ( 'NONE', *, *, #3925, .T. ) ;
#2191 = FACE_BOUND ( 'NONE', #7342, .T. ) ;
#2192 = PRODUCT_DEFINITION_SHAPE ( 'NONE', 'NONE',  #8612 ) ;
#2193 = DIRECTION ( 'NONE',  ( 1.000000000000000000, 0.000000000000000000, 0.000000000000000000 ) ) ;
#2194 = ADVANCED_FACE ( 'NONE', ( #2338 ), #584, .F. ) ;
#2195 = DIRECTION ( 'NONE',  ( 0.000000000000000000, 0.000000000000000000, -1.000000000000000000 ) ) ;
#2196 = MECHANICAL_DESIGN_GEOMETRIC_PRESENTATION_REPRESENTATION (  '', ( #6917 ), #5930 ) ;
#2197 = DIRECTION ( 'NONE',  ( 1.000000000000000000, 0.000000000000000000, 0.000000000000000000 ) ) ;
#2198 = CARTESIAN_POINT ( 'NONE',  ( -1.390230914382372118, -4.043987460488664532, -3.502507215260523665 ) ) ;
#2199 = CARTESIAN_POINT ( 'NONE',  ( 0.000000000000000000, 1.178949249685213863, -2.042000000000001148 ) ) ;
#2200 = VERTEX_POINT ( 'NONE', #5960 ) ;
#2201 = VERTEX_POINT ( 'NONE', #8552 ) ;
#2202 = EDGE_LOOP ( 'NONE', ( #32, #7144, #1467, #5379 ) ) ;
#2203 = DIRECTION ( 'NONE',  ( -1.000000000000000000, -0.000000000000000000, -0.000000000000000000 ) ) ;
#2204 = ORIENTED_EDGE ( 'NONE', *, *, #6722, .T. ) ;
#2205 = FACE_OUTER_BOUND ( 'NONE', #2168, .T. ) ;
#2206 = EDGE_CURVE ( 'NONE', #8570, #342, #3160, .T. ) ;
#2207 = VERTEX_POINT ( 'NONE', #2135 ) ;
#2208 = CARTESIAN_POINT ( 'NONE',  ( -6.473970235329672780E-16, -4.862606272033106691, -3.745885042887442395 ) ) ;
#2209 = DIRECTION ( 'NONE',  ( 0.000000000000000000, 1.000000000000000000, 0.000000000000000000 ) ) ;
#2210 = EDGE_CURVE ( 'NONE', #863, #3178, #6618, .T. ) ;
#2211 = FILL_AREA_STYLE_COLOUR ( '', #6693 ) ;
#2212 = ORIENTED_EDGE ( 'NONE', *, *, #1197, .F. ) ;
#2213 = ORIENTED_EDGE ( 'NONE', *, *, #5279, .T. ) ;
#2214 = DIRECTION ( 'NONE',  ( 1.000000000000000000, 0.000000000000000000, 0.000000000000000000 ) ) ;
#2215 = AXIS2_PLACEMENT_3D ( 'NONE', #112, #6170, #204 ) ;
#2216 = ADVANCED_FACE ( 'NONE', ( #4618 ), #2509, .T. ) ;
#2217 = CARTESIAN_POINT ( 'NONE',  ( -6.473970235329672780E-16, -4.862606272033106691, -3.745885042887442395 ) ) ;
#2218 = CARTESIAN_POINT ( 'NONE',  ( -0.6920835326022555245, -4.454600218803899558, -3.597382984111586079 ) ) ;
#2219 = AXIS2_PLACEMENT_3D ( 'NONE', #6315, #2882, #4843 ) ;
#2220 = CARTESIAN_POINT ( 'NONE',  ( 3.455068668934414777, -2.624017327439094327, -3.316620875263732504 ) ) ;
#2221 = VERTEX_POINT ( 'NONE', #1193 ) ;
#2222 = SURFACE_SIDE_STYLE ('',( #3442 ) ) ;
#2223 = CARTESIAN_POINT ( 'NONE',  ( 0.000000000000000000, 0.000000000000000000, -0.3080913168122742518 ) ) ;
#2224 = ORIENTED_EDGE ( 'NONE', *, *, #758, .F. ) ;
#2225 = ORIENTED_EDGE ( 'NONE', *, *, #3672, .F. ) ;
#2226 = CARTESIAN_POINT ( 'NONE',  ( 5.200000000000002842, 0.000000000000000000, 0.000000000000000000 ) ) ;
#2227 = CARTESIAN_POINT ( 'NONE',  ( -5.000000000000000000, -5.000000000000000000, 148.0000000000000284 ) ) ;
#2228 = VECTOR ( 'NONE', #1104, 1000.000000000000000 ) ;
#2229 = EDGE_CURVE ( 'NONE', #4164, #3505, #516, .T. ) ;
#2230 = DIRECTION ( 'NONE',  ( -1.734723475976806848E-16, 1.000000000000000000, 0.000000000000000000 ) ) ;
#2231 = CARTESIAN_POINT ( 'NONE',  ( -2.000000000000007550, -3.464101615137749945, 0.000000000000000000 ) ) ;
#2232 = ORIENTED_EDGE ( 'NONE', *, *, #3645, .F. ) ;
#2233 = CARTESIAN_POINT ( 'NONE',  ( -0.3461262719736137305, 4.658553426539289610, -3.671615880910373608 ) ) ;
#2234 = AXIS2_PLACEMENT_3D ( 'NONE', #3612, #384, #8364 ) ;
#2235 =( NAMED_UNIT ( * ) PLANE_ANGLE_UNIT ( ) SI_UNIT ( $, .RADIAN. ) );
#2236 = DIRECTION ( 'NONE',  ( 0.000000000000000000, 0.000000000000000000, 1.000000000000000000 ) ) ;
#2237 = LINE ( 'NONE', #6361, #2813 ) ;
#2238 = CARTESIAN_POINT ( 'NONE',  ( 93.00000000000000000, -4.999999999999998224, 140.0000000000000000 ) ) ;
#2239 = DIRECTION ( 'NONE',  ( -1.734723475976806848E-16, 1.000000000000000000, 0.000000000000000000 ) ) ;
#2240 = LINE ( 'NONE', #2199, #2737 ) ;
#2241 = EDGE_LOOP ( 'NONE', ( #6031, #2559, #1085, #3839 ) ) ;
#2242 = ORIENTED_EDGE ( 'NONE', *, *, #6880, .T. ) ;
#2243 = CARTESIAN_POINT ( 'NONE',  ( 4.000000000000000000, -2.309401076758516691, -0.4999999999999995559 ) ) ;
#2244 = MANIFOLD_SOLID_BREP ( 'Boss-Extrude4', #1478 ) ;
#2245 = DIRECTION ( 'NONE',  ( -0.000000000000000000, 1.000000000000000000, -0.000000000000000000 ) ) ;
#2246 = COLOUR_RGB ( '',0.8941176470588234615, 0.8941176470588234615, 0.8941176470588234615 ) ;
#2247 = ORIENTED_EDGE ( 'NONE', *, *, #1992, .T. ) ;
#2248 = DIRECTION ( 'NONE',  ( -0.000000000000000000, -0.000000000000000000, -1.000000000000000000 ) ) ;
#2249 = VERTEX_POINT ( 'NONE', #8594 ) ;
#2250 = DIRECTION ( 'NONE',  ( 1.000000000000000000, 0.000000000000000000, 0.000000000000000000 ) ) ;
#2251 = APPLICATION_CONTEXT ( 'automotive_design' ) ;
#2252 = CARTESIAN_POINT ( 'NONE',  ( -5.000000000000001776, 5.000000000000001776, 148.0000000000000284 ) ) ;
#2253 = ITEM_DEFINED_TRANSFORMATION ( 'NONE', 'NONE', #8089,  #594 ) ;
#2254 = DIRECTION ( 'NONE',  ( 0.000000000000000000, 0.000000000000000000, -1.000000000000000000 ) ) ;
#2255 = VERTEX_POINT ( 'NONE', #5832 ) ;
#2256 = EDGE_CURVE ( 'NONE', #5747, #5984, #1935, .T. ) ;
#2257 = EDGE_LOOP ( 'NONE', ( #2935, #6507, #7530, #2667 ) ) ;
#2258 = AXIS2_PLACEMENT_3D ( 'NONE', #5042, #7712, #5812 ) ;
#2259 = CARTESIAN_POINT ( 'NONE',  ( 303.3333333333333144, -20.00000000000000000, 159.8500000000001080 ) ) ;
#2260 = VECTOR ( 'NONE', #7986, 1000.000000000000000 ) ;
#2261 = CARTESIAN_POINT ( 'NONE',  ( -1.999999999999999556, 3.464101615137754830, -3.142992957459232795 ) ) ;
#2262 = ADVANCED_FACE ( 'NONE', ( #3321 ), #8505, .F. ) ;
#2263 = MANIFOLD_SOLID_BREP ( 'Cut-Extrude1', #4113 ) ;
#2264 = VECTOR ( 'NONE', #8036, 1000.000000000000000 ) ;
#2265 = EDGE_CURVE ( 'NONE', #4949, #2181, #6120, .T. ) ;
#2266 = CARTESIAN_POINT ( 'NONE',  ( 181.0000000000000000, -4.999999999999998224, 139.9990000000000236 ) ) ;
#2267 = EDGE_LOOP ( 'NONE', ( #5425, #7201 ) ) ;
#2268 = DIRECTION ( 'NONE',  ( 1.734723475976807341E-16, 0.000000000000000000, -1.000000000000000000 ) ) ;
#2269 = ORIENTED_EDGE ( 'NONE', *, *, #1199, .T. ) ;
#2270 = VECTOR ( 'NONE', #1930, 1000.000000000000000 ) ;
#2271 = EDGE_CURVE ( 'NONE', #6071, #7348, #1853, .T. ) ;
#2272 =( NAMED_UNIT ( * ) PLANE_ANGLE_UNIT ( ) SI_UNIT ( $, .RADIAN. ) );
#2273 = CARTESIAN_POINT ( 'NONE',  ( 0.000000000000000000, 0.000000000000000000, 3.469446951953614189E-15 ) ) ;
#2274 = EDGE_LOOP ( 'NONE', ( #4630, #7257, #2639, #7405 ) ) ;
#2275 = CARTESIAN_POINT ( 'NONE',  ( -1.360585162435467455, 4.061296242128285883, -3.505054077164959203 ) ) ;
#2276 = FACE_BOUND ( 'NONE', #851, .T. ) ;
#2277 = VECTOR ( 'NONE', #5213, 1000.000000000000000 ) ;
#2278 = AXIS2_PLACEMENT_3D ( 'NONE', #5863, #6593, #2565 ) ;
#2279 = VECTOR ( 'NONE', #6025, 1000.000000000000000 ) ;
#2280 = CARTESIAN_POINT ( 'NONE',  ( 3.678949249685231848, 0.000000000000000000, 0.000000000000000000 ) ) ;
#2281 = PLANE ( 'NONE',  #4149 ) ;
#2282 = ORIENTED_EDGE ( 'NONE', *, *, #4122, .T. ) ;
#2283 = LINE ( 'NONE', #4929, #263 ) ;
#2284 = VECTOR ( 'NONE', #2214, 1000.000000000000000 ) ;
#2285 = CARTESIAN_POINT ( 'NONE',  ( 0.000000000000000000, 0.000000000000000000, -43.99999999999997158 ) ) ;
#2286 = VECTOR ( 'NONE', #8261, 1000.000000000000000 ) ;
#2287 = DIRECTION ( 'NONE',  ( 0.000000000000000000, -0.4999999999999992784, 0.8660254037844389297 ) ) ;
#2288 = AXIS2_PLACEMENT_3D ( 'NONE', #2049, #2653, #7966 ) ;
#2289 = CARTESIAN_POINT ( 'NONE',  ( 5.000000000000000000, 5.000000000000000000, -97.99999999999997158 ) ) ;
#2290 = LINE ( 'NONE', #4934, #2510 ) ;
#2291 = DIRECTION ( 'NONE',  ( 0.000000000000000000, 0.4999999999999993339, -0.8660254037844390407 ) ) ;
#2292 = AXIS2_PLACEMENT_3D ( 'NONE', #1938, #5922, #2512 ) ;
#2293 = ORIENTED_EDGE ( 'NONE', *, *, #7855, .T. ) ;
#2294 = ORIENTED_EDGE ( 'NONE', *, *, #7291, .T. ) ;
#2295 = EDGE_CURVE ( 'NONE', #1754, #3213, #6782, .T. ) ;
#2296 = EDGE_CURVE ( 'NONE', #4980, #832, #2754, .T. ) ;
#2297 = EDGE_LOOP ( 'NONE', ( #6653, #3730, #6017 ) ) ;
#2298 = DIRECTION ( 'NONE',  ( -1.000000000000000000, 0.000000000000000000, 0.000000000000000000 ) ) ;
#2299 = EDGE_CURVE ( 'NONE', #3347, #4177, #3888, .T. ) ;
#2300 = CARTESIAN_POINT ( 'NONE',  ( -5.000000000000001776, 5.000000000000001776, 140.0000000000000000 ) ) ;
#2301 = AXIS2_PLACEMENT_3D ( 'NONE', #8518, #1242, #6546 ) ;
#2302 = B_SPLINE_CURVE_WITH_KNOTS ( 'NONE', 3,
 ( #1945, #3078, #3248, #4505, #6422, #4586, #5721, #465 ),
 .UNSPECIFIED., .F., .F.,
 ( 4, 2, 2, 4 ),
 ( 0.005725059856848641743, 0.006314084072593626612, 0.006903108288338611481, 0.008081156719828581220 ),
 .UNSPECIFIED. ) ;
#2303 = VERTEX_POINT ( 'NONE', #5226 ) ;
#2304 = CARTESIAN_POINT ( 'NONE',  ( 470.0000000000000000, -20.00000000000000000, 200.0000000000000000 ) ) ;
#2305 = ORIENTED_EDGE ( 'NONE', *, *, #7524, .F. ) ;
#2306 = CARTESIAN_POINT ( 'NONE',  ( 107.9310344827585908, -25.00000000000000000, -144.8275862068965125 ) ) ;
#2307 = CARTESIAN_POINT ( 'NONE',  ( -5.000000000000001776, 5.000000000000001776, -71.99999999999998579 ) ) ;
#2308 = ORIENTED_EDGE ( 'NONE', *, *, #5103, .T. ) ;
#2309 = ORIENTED_EDGE ( 'NONE', *, *, #2271, .F. ) ;
#2310 = CARTESIAN_POINT ( 'NONE',  ( 176.0000000000000000, -20.00000000000000000, -83.98142504031548583 ) ) ;
#2311 = EDGE_CURVE ( 'NONE', #716, #5369, #4748, .T. ) ;
#2312 = DIRECTION ( 'NONE',  ( -1.000000000000000000, -0.000000000000000000, -0.000000000000000000 ) ) ;
#2313 = APPLICATION_CONTEXT ( 'automotive_design' ) ;
#2314 = FACE_OUTER_BOUND ( 'NONE', #3354, .T. ) ;
#2315 = DIRECTION ( 'NONE',  ( 0.000000000000000000, 0.000000000000000000, 1.000000000000000000 ) ) ;
#2316 = EDGE_LOOP ( 'NONE', ( #7296, #407, #8302, #7762 ) ) ;
#2317 = PRESENTATION_STYLE_ASSIGNMENT (( #3611 ) ) ;
#2318 = CARTESIAN_POINT ( 'NONE',  ( 357.0000000000000000, -4.999999999999998224, 139.9990000000000236 ) ) ;
#2319 = ORIENTED_EDGE ( 'NONE', *, *, #6075, .F. ) ;
#2320 = ORIENTED_EDGE ( 'NONE', *, *, #5595, .T. ) ;
#2321 = CIRCLE ( 'NONE', #5352, 2.649999999999985700 ) ;
#2322 = CARTESIAN_POINT ( 'NONE',  ( 0.000000000000000000, 0.000000000000000000, -77.99999999999997158 ) ) ;
#2323 = FACE_OUTER_BOUND ( 'NONE', #4142, .T. ) ;
#2324 = ADVANCED_FACE ( 'NONE', ( #752 ), #2017, .F. ) ;
#2325 = VECTOR ( 'NONE', #5417, 1000.000000000000000 ) ;
#2326 = DIRECTION ( 'NONE',  ( 0.000000000000000000, 0.000000000000000000, 1.000000000000000000 ) ) ;
#2327 = CIRCLE ( 'NONE', #3563, 4.000000000000000000 ) ;
#2328 = DIRECTION ( 'NONE',  ( 1.734723475976806848E-16, -1.000000000000000000, -0.000000000000000000 ) ) ;
#2329 = ORIENTED_EDGE ( 'NONE', *, *, #6482, .T. ) ;
#2330 = DIRECTION ( 'NONE',  ( -0.000000000000000000, -0.000000000000000000, -1.000000000000000000 ) ) ;
#2331 = ORIENTED_EDGE ( 'NONE', *, *, #7096, .T. ) ;
#2332 = CARTESIAN_POINT ( 'NONE',  ( -3.349226789952655547, -2.685125164760744809, -0.2236248678334863682 ) ) ;
#2333 = AXIS2_PLACEMENT_3D ( 'NONE', #443, #1849, #4449 ) ;
#2334 = ADVANCED_FACE ( 'NONE', ( #7889, #8074 ), #6047, .T. ) ;
#2335 = CARTESIAN_POINT ( 'NONE',  ( 0.000000000000000000, 0.000000000000000000, -71.99999999999998579 ) ) ;
#2336 = CARTESIAN_POINT ( 'NONE',  ( -30.00000000000002842, -25.00000000000000000, 200.0000000000000000 ) ) ;
#2337 = CARTESIAN_POINT ( 'NONE',  ( -4.235886605889389145, -2.417314728048544303, -3.751161874094020909 ) ) ;
#2338 = FACE_OUTER_BOUND ( 'NONE', #2029, .T. ) ;
#2339 = EDGE_LOOP ( 'NONE', ( #3332, #2695, #2341, #6159 ) ) ;
#2340 = ORIENTED_EDGE ( 'NONE', *, *, #8248, .T. ) ;
#2341 = ORIENTED_EDGE ( 'NONE', *, *, #2411, .F. ) ;
#2342 = CARTESIAN_POINT ( 'NONE',  ( -30.00000000000002842, -15.00000000000000000, 145.0000000000000284 ) ) ;
#2343 = DIRECTION ( 'NONE',  ( -0.000000000000000000, 1.000000000000000000, -0.000000000000000000 ) ) ;
#2344 = PRODUCT_DEFINITION_SHAPE ( 'NONE', 'NONE',  #8633 ) ;
#2345 = EDGE_CURVE ( 'NONE', #1959, #5488, #1265, .T. ) ;
#2346 = EDGE_LOOP ( 'NONE', ( #2224, #7035, #3120 ) ) ;
#2347 = CARTESIAN_POINT ( 'NONE',  ( 0.000000000000000000, -25.00000000000000000, -157.5000000000000284 ) ) ;
#2348 = AXIS2_PLACEMENT_3D ( 'NONE', #2098, #7274, #4571 ) ;
#2349 = VERTEX_POINT ( 'NONE', #3236 ) ;
#2350 = FACE_OUTER_BOUND ( 'NONE', #6123, .T. ) ;
#2351 = CONTEXT_DEPENDENT_SHAPE_REPRESENTATION ( #2752, #6841 ) ;
#2352 = EDGE_LOOP ( 'NONE', ( #7732, #7134, #4112, #7783 ) ) ;
#2353 = EDGE_LOOP ( 'NONE', ( #3218, #4790, #5597, #7120 ) ) ;
#2354 = DIRECTION ( 'NONE',  ( -1.000000000000000000, 0.000000000000000000, -0.000000000000000000 ) ) ;
#2355 = CARTESIAN_POINT ( 'NONE',  ( -5.000000000000000000, -5.000000000000000000, 140.0000000000000000 ) ) ;
#2356 = CARTESIAN_POINT ( 'NONE',  ( 4.197393957002303999, -0.4069871074557456780, -3.503767560748925813 ) ) ;
#2357 = CARTESIAN_POINT ( 'NONE',  ( 352.0000000000000000, -25.00000000000000000, -16.23142504031546807 ) ) ;
#2358 = ORIENTED_EDGE ( 'NONE', *, *, #6509, .T. ) ;
#2359 = CARTESIAN_POINT ( 'NONE',  ( 303.3333333333333144, -10.00000000000000000, 162.5000000000000853 ) ) ;
#2360 = LINE ( 'NONE', #1702, #5318 ) ;
#2361 = ORIENTED_EDGE ( 'NONE', *, *, #5807, .T. ) ;
#2362 = ORIENTED_EDGE ( 'NONE', *, *, #378, .F. ) ;
#2363 = CARTESIAN_POINT ( 'NONE',  ( 444.9999999999999432, -4.999999999999998224, 139.9990000000000236 ) ) ;
#2364 = DIRECTION ( 'NONE',  ( 0.000000000000000000, -1.000000000000000000, 1.287488025362403787E-15 ) ) ;
#2365 = VECTOR ( 'NONE', #5347, 1000.000000000000000 ) ;
#2366 = PLANE ( 'NONE',  #4409 ) ;
#2367 = CARTESIAN_POINT ( 'NONE',  ( 357.0000000000000000, -4.999999999999998224, 139.9990000000000236 ) ) ;
#2368 = ORIENTED_EDGE ( 'NONE', *, *, #2025, .F. ) ;
#2369 = FACE_OUTER_BOUND ( 'NONE', #2058, .T. ) ;
#2370 = ORIENTED_EDGE ( 'NONE', *, *, #5126, .F. ) ;
#2371 = VECTOR ( 'NONE', #1631, 1000.000000000000000 ) ;
#2372 = DIRECTION ( 'NONE',  ( -0.000000000000000000, -0.000000000000000000, 1.000000000000000000 ) ) ;
#2373 = CARTESIAN_POINT ( 'NONE',  ( 2.500000000000000000, -2.357898499370432610, 3.252606517456513302E-15 ) ) ;
#2374 = EDGE_CURVE ( 'NONE', #6072, #3976, #1311, .T. ) ;
#2375 = EDGE_CURVE ( 'NONE', #238, #24, #4015, .T. ) ;
#2376 = AXIS2_PLACEMENT_3D ( 'NONE', #4715, #1275, #6584 ) ;
#2377 = CARTESIAN_POINT ( 'NONE',  ( 20.00000000000000000, 175.0000000000000284, 5.000000000000000000 ) ) ;
#2378 = EDGE_CURVE ( 'NONE', #798, #1337, #8326, .T. ) ;
#2379 = AXIS2_PLACEMENT_3D ( 'NONE', #3993, #4590, #2600 ) ;
#2380 = CARTESIAN_POINT ( 'NONE',  ( -2.836893136758495970, -3.208949435745868328, -3.505054077164885484 ) ) ;
#2381 = CARTESIAN_POINT ( 'NONE',  ( -4.000000000000000000, -2.472261339043343220, -3.687027428081192326 ) ) ;
#2382 = VERTEX_POINT ( 'NONE', #6573 ) ;
#2383 = EDGE_CURVE ( 'NONE', #5788, #1426, #7404, .T. ) ;
#2384 = ORIENTED_EDGE ( 'NONE', *, *, #6116, .F. ) ;
#2385 = CARTESIAN_POINT ( 'NONE',  ( 2.687328764639642653, -3.067272167851299969, -0.05923475698271395140 ) ) ;
#2386 = LINE ( 'NONE', #3763, #43 ) ;
#2387 = DIRECTION ( 'NONE',  ( -1.000000000000000000, 0.000000000000000000, -0.000000000000000000 ) ) ;
#2388 = UNCERTAINTY_MEASURE_WITH_UNIT (LENGTH_MEASURE( 1.000000000000000082E-05 ), #2179, 'distance_accuracy_value', 'NONE');
#2389 = VERTEX_POINT ( 'NONE', #8550 ) ;
#2390 =( LENGTH_UNIT ( ) NAMED_UNIT ( * ) SI_UNIT ( .MILLI., .METRE. ) );
#2391 = ORIENTED_EDGE ( 'NONE', *, *, #7367, .T. ) ;
#2392 = DIRECTION ( 'NONE',  ( -0.000000000000000000, -0.000000000000000000, -1.000000000000000000 ) ) ;
#2393 = ITEM_DEFINED_TRANSFORMATION ( 'NONE', 'NONE', #1415,  #594 ) ;
#2394 = ORIENTED_EDGE ( 'NONE', *, *, #1790, .T. ) ;
#2395 = ORIENTED_EDGE ( 'NONE', *, *, #666, .T. ) ;
#2396 = EDGE_CURVE ( 'NONE', #7425, #337, #6657, .T. ) ;
#2397 = CARTESIAN_POINT ( 'NONE',  ( 470.0000000000000000, -20.00000000000000000, 180.0000000000000284 ) ) ;
#2398 = DIRECTION ( 'NONE',  ( -1.000000000000000000, 0.000000000000000000, -0.000000000000000000 ) ) ;
#2399 = CARTESIAN_POINT ( 'NONE',  ( 3.999999999999999112, -1.539600717839012978, -3.300726591567080703 ) ) ;
#2400 = DIRECTION ( 'NONE',  ( -0.000000000000000000, 1.000000000000000000, -0.000000000000000000 ) ) ;
#2401 = EDGE_LOOP ( 'NONE', ( #2161, #1516, #1755, #3546 ) ) ;
#2402 = CARTESIAN_POINT ( 'NONE',  ( 0.000000000000000000, 0.000000000000000000, -25.03750572909317285 ) ) ;
#2403 = CARTESIAN_POINT ( 'NONE',  ( 136.6666666666666288, -30.00000000000000355, 162.5000000000000853 ) ) ;
#2404 = CARTESIAN_POINT ( 'NONE',  ( 170.9999999999999716, 5.000000000000001776, 145.0000000000000284 ) ) ;
#2405 = ORIENTED_EDGE ( 'NONE', *, *, #6103, .T. ) ;
#2406 = VERTEX_POINT ( 'NONE', #5876 ) ;
#2407 = EDGE_CURVE ( 'NONE', #101, #6809, #701, .T. ) ;
#2408 = DIRECTION ( 'NONE',  ( -1.000000000000000000, 0.000000000000000000, 0.000000000000000000 ) ) ;
#2409 = EDGE_CURVE ( 'NONE', #2174, #3740, #7888, .T. ) ;
#2410 = CARTESIAN_POINT ( 'NONE',  ( -4.999999999999998224, -4.999999999999998224, 145.0000000000000284 ) ) ;
#2411 = EDGE_CURVE ( 'NONE', #5372, #8533, #2622, .T. ) ;
#2412 = AXIS2_PLACEMENT_3D ( 'NONE', #1888, #7058, #4406 ) ;
#2413 = CARTESIAN_POINT ( 'NONE',  ( 0.000000000000000000, 0.000000000000000000, 120.0000000000000142 ) ) ;
#2414 = DIRECTION ( 'NONE',  ( 0.000000000000000000, 0.000000000000000000, 1.000000000000000000 ) ) ;
#2415 = VERTEX_POINT ( 'NONE', #7934 ) ;
#2416 = TOROIDAL_SURFACE ( 'NONE', #6431, 4.000000000000000000, 0.2500000000000000000 ) ;
#2417 =( NAMED_UNIT ( * ) PLANE_ANGLE_UNIT ( ) SI_UNIT ( $, .RADIAN. ) );
#2418 = ORIENTED_EDGE ( 'NONE', *, *, #6429, .T. ) ;
#2419 = VECTOR ( 'NONE', #7477, 1000.000000000000000 ) ;
#2420 = CARTESIAN_POINT ( 'NONE',  ( 0.000000000000000000, 0.000000000000000000, -143.0000000000000284 ) ) ;
#2421 = AXIS2_PLACEMENT_3D ( 'NONE', #1091, #6309, #4310 ) ;
#2422 = DIRECTION ( 'NONE',  ( 0.000000000000000000, 0.000000000000000000, 1.000000000000000000 ) ) ;
#2423 = CARTESIAN_POINT ( 'NONE',  ( 264.0000000000000000, -25.00000000000000000, -54.08142504031544462 ) ) ;
#2424 = LINE ( 'NONE', #3193, #2926 ) ;
#2425 = CIRCLE ( 'NONE', #7129, 10.00000000000000000 ) ;
#2426 = CARTESIAN_POINT ( 'NONE',  ( 0.000000000000000000, 0.000000000000000000, -115.0000000000000000 ) ) ;
#2427 = DIRECTION ( 'NONE',  ( -0.000000000000000000, -0.000000000000000000, 1.000000000000000000 ) ) ;
#2428 = VERTEX_POINT ( 'NONE', #1970 ) ;
#2429 = AXIS2_PLACEMENT_3D ( 'NONE', #810, #6720, #232 ) ;
#2430 = MECHANICAL_DESIGN_GEOMETRIC_PRESENTATION_REPRESENTATION (  '', ( #4916 ), #2698 ) ;
#2431 = CARTESIAN_POINT ( 'NONE',  ( 10.00000000000000000, 0.000000000000000000, -97.99999999999997158 ) ) ;
#2432 = DIRECTION ( 'NONE',  ( 1.000000000000000000, 0.000000000000000000, 0.000000000000000000 ) ) ;
#2433 = DIRECTION ( 'NONE',  ( -1.000000000000000000, 1.734723475976806848E-16, -0.000000000000000000 ) ) ;
#2434 =( REPRESENTATION_RELATIONSHIP ('NONE','NONE', #3312, #872 ) REPRESENTATION_RELATIONSHIP_WITH_TRANSFORMATION ( #327 )SHAPE_REPRESENTATION_RELATIONSHIP( ) );
#2435 = EDGE_CURVE ( 'NONE', #3488, #2469, #8028, .T. ) ;
#2436 = VECTOR ( 'NONE', #5675, 1000.000000000000000 ) ;
#2437 = ORIENTED_EDGE ( 'NONE', *, *, #5827, .F. ) ;
#2438 = DIRECTION ( 'NONE',  ( -1.000000000000000000, 0.000000000000000000, 0.000000000000000000 ) ) ;
#2439 = ORIENTED_EDGE ( 'NONE', *, *, #5785, .F. ) ;
#2440 = DIRECTION ( 'NONE',  ( 0.000000000000000000, 0.000000000000000000, -1.000000000000000000 ) ) ;
#2441 = EDGE_LOOP ( 'NONE', ( #5332, #8168 ) ) ;
#2442 = ORIENTED_EDGE ( 'NONE', *, *, #5342, .F. ) ;
#2443 = VECTOR ( 'NONE', #2576, 1000.000000000000000 ) ;
#2444 = FACE_OUTER_BOUND ( 'NONE', #4566, .T. ) ;
#2445 = CARTESIAN_POINT ( 'NONE',  ( 259.0000000000000000, -4.999999999999998224, 140.0000000000000000 ) ) ;
#2446 = CYLINDRICAL_SURFACE ( 'NONE', #5223, 2.649999999999985700 ) ;
#2447 = EDGE_LOOP ( 'NONE', ( #4684, #602, #95, #7172 ) ) ;
#2448 = DIRECTION ( 'NONE',  ( 1.000000000000000000, 0.000000000000000000, 0.000000000000000000 ) ) ;
#2449 = CARTESIAN_POINT ( 'NONE',  ( 303.3333333333333144, -20.00000000000000000, 162.5000000000000853 ) ) ;
#2450 = ORIENTED_EDGE ( 'NONE', *, *, #8409, .T. ) ;
#2451 = VERTEX_POINT ( 'NONE', #4053 ) ;
#2452 = CARTESIAN_POINT ( 'NONE',  ( -5.000000000000001776, 5.000000000000001776, -63.99999999999997158 ) ) ;
#2453 = CARTESIAN_POINT ( 'NONE',  ( 4.000000000000000000, -2.309401076758514915, -3.433295621305383349 ) ) ;
#2454 = PLANE ( 'NONE',  #1195 ) ;
#2455 = ADVANCED_FACE ( 'NONE', ( #4615 ), #6615, .F. ) ;
#2456 = CYLINDRICAL_SURFACE ( 'NONE', #6925, 10.00000000000000000 ) ;
#2457 = ORIENTED_EDGE ( 'NONE', *, *, #7174, .F. ) ;
#2458 = EDGE_CURVE ( 'NONE', #7520, #3184, #2755, .T. ) ;
#2459 = AXIS2_PLACEMENT_3D ( 'NONE', #5476, #2909, #8231 ) ;
#2460 = APPLICATION_PROTOCOL_DEFINITION ( 'draft international standard', 'automotive_design', 1998, #7470 ) ;
#2461 = ORIENTED_EDGE ( 'NONE', *, *, #4826, .F. ) ;
#2462 = FACE_OUTER_BOUND ( 'NONE', #4150, .T. ) ;
#2463 = VECTOR ( 'NONE', #7868, 1000.000000000000000 ) ;
#2464 = FACE_OUTER_BOUND ( 'NONE', #4631, .T. ) ;
#2465 = CARTESIAN_POINT ( 'NONE',  ( 5.000000000000000000, -5.000000000000000000, 148.0000000000000284 ) ) ;
#2466 = DIRECTION ( 'NONE',  ( -0.000000000000000000, -0.000000000000000000, 1.000000000000000000 ) ) ;
#2467 =( NAMED_UNIT ( * ) PLANE_ANGLE_UNIT ( ) SI_UNIT ( $, .RADIAN. ) );
#2469 = VERTEX_POINT ( 'NONE', #3494 ) ;
#2468 = EDGE_CURVE ( 'NONE', #884, #6060, #7909, .T. ) ;
#2470 = AXIS2_PLACEMENT_3D ( 'NONE', #5762, #6331, #3162 ) ;
#2471 = CLOSED_SHELL ( 'NONE', ( #7255, #7833, #6353, #5712, #412, #2712, #6984, #1459, #4194, #2036, #5069, #6579, #90, #4652, #5361, #6607, #7854, #8488, #2888, #4408 ) ) ;
#2472 = PRESENTATION_STYLE_ASSIGNMENT (( #5191 ) ) ;
#2473 = LINE ( 'NONE', #1231, #6450 ) ;
#2474 = DIRECTION ( 'NONE',  ( -0.000000000000000000, -0.000000000000000000, 1.000000000000000000 ) ) ;
#2475 = CIRCLE ( 'NONE', #8167, 10.00000000000000000 ) ;
#2476 = ORIENTED_EDGE ( 'NONE', *, *, #953, .F. ) ;
#2477 = EDGE_LOOP ( 'NONE', ( #1736, #6913, #190, #4003 ) ) ;
#2478 =( NAMED_UNIT ( * ) PLANE_ANGLE_UNIT ( ) SI_UNIT ( $, .RADIAN. ) );
#2479 = DIRECTION ( 'NONE',  ( -1.000000000000000000, 0.000000000000000000, 0.000000000000000000 ) ) ;
#2480 = CONTEXT_DEPENDENT_SHAPE_REPRESENTATION ( #4973, #5848 ) ;
#2481 = ORIENTED_EDGE ( 'NONE', *, *, #7318, .T. ) ;
#2482 = EDGE_LOOP ( 'NONE', ( #6513, #1685, #1592 ) ) ;
#2483 = CARTESIAN_POINT ( 'NONE',  ( 2.500000000000000888, 3.061616997868384127E-16, -4.974599999999998801 ) ) ;
#2484 = DIRECTION ( 'NONE',  ( 0.000000000000000000, 1.000000000000000000, 0.000000000000000000 ) ) ;
#2485 = EDGE_CURVE ( 'NONE', #1044, #3408, #168, .T. ) ;
#2486 = VECTOR ( 'NONE', #5399, 1000.000000000000000 ) ;
#2487 = CARTESIAN_POINT ( 'NONE',  ( -4.000000000000000000, -2.309401076758515803, -0.4999999999999995559 ) ) ;
#2488 = EDGE_CURVE ( 'NONE', #5639, #7425, #3535, .T. ) ;
#2489 = ORIENTED_EDGE ( 'NONE', *, *, #2378, .F. ) ;
#2490 = DIRECTION ( 'NONE',  ( 1.000000000000000000, 6.123233995736766036E-17, -6.123233995736764803E-17 ) ) ;
#2491 = FACE_BOUND ( 'NONE', #4114, .T. ) ;
#2492 = EDGE_LOOP ( 'NONE', ( #7476, #3168, #5507, #6785 ) ) ;
#2493 = EDGE_CURVE ( 'NONE', #1782, #7349, #2839, .T. ) ;
#2494 = ORIENTED_EDGE ( 'NONE', *, *, #5666, .F. ) ;
#2495 = DIRECTION ( 'NONE',  ( 0.000000000000000000, -0.5000000000000011102, -0.8660254037844379305 ) ) ;
#2496 = CARTESIAN_POINT ( 'NONE',  ( 0.000000000000000000, 2.357898499370433054, -1.951563910473907981E-15 ) ) ;
#2497 = FACE_OUTER_BOUND ( 'NONE', #1636, .T. ) ;
#2498 = AXIS2_PLACEMENT_3D ( 'NONE', #2499, #4483, #526 ) ;
#2499 = CARTESIAN_POINT ( 'NONE',  ( -5.000000000000000000, -5.000000000000000000, -105.9999999999999858 ) ) ;
#2500 = VERTEX_POINT ( 'NONE', #8156 ) ;
#2501 = ORIENTED_EDGE ( 'NONE', *, *, #8465, .T. ) ;
#2502 = CARTESIAN_POINT ( 'NONE',  ( 0.6810597143197052450, 4.461075778259290914, -3.598441714920602053 ) ) ;
#2503 = EDGE_CURVE ( 'NONE', #2451, #3613, #968, .T. ) ;
#2504 = AXIS2_PLACEMENT_3D ( 'NONE', #1320, #2069, #7371 ) ;
#2505 = ADVANCED_FACE ( 'NONE', ( #5529 ), #2146, .T. ) ;
#2506 = DIRECTION ( 'NONE',  ( 0.000000000000000000, -0.000000000000000000, 1.000000000000000000 ) ) ;
#2507 = DIRECTION ( 'NONE',  ( 1.000000000000000000, 0.000000000000000000, -0.000000000000000000 ) ) ;
#2508 = CARTESIAN_POINT ( 'NONE',  ( 10.00000000000000000, 0.000000000000000000, -97.99999999999997158 ) ) ;
#2509 = CYLINDRICAL_SURFACE ( 'NONE', #7752, 10.00000000000000000 ) ;
#2510 = VECTOR ( 'NONE', #8253, 1000.000000000000000 ) ;
#2511 = DIRECTION ( 'NONE',  ( 1.000000000000000000, -1.734723475976806848E-16, 0.000000000000000000 ) ) ;
#2512 = DIRECTION ( 'NONE',  ( 0.000000000000000000, 0.000000000000000000, 1.000000000000000000 ) ) ;
#2513 = LINE ( 'NONE', #7988, #1153 ) ;
#2514 = VECTOR ( 'NONE', #2846, 1000.000000000000000 ) ;
#2515 = DIRECTION ( 'NONE',  ( 1.000000000000000000, -1.734723475976806848E-16, 0.000000000000000000 ) ) ;
#2516 = ORIENTED_EDGE ( 'NONE', *, *, #5862, .T. ) ;
#2517 = DIRECTION ( 'NONE',  ( 0.000000000000000000, 1.000000000000000000, 0.000000000000000000 ) ) ;
#2518 = VECTOR ( 'NONE', #1659, 1000.000000000000000 ) ;
#2519 = ORIENTED_EDGE ( 'NONE', *, *, #3228, .T. ) ;
#2520 = CARTESIAN_POINT ( 'NONE',  ( 5.000000000000000000, -5.000000000000000000, -0.9999999999999940048 ) ) ;
#2521 = CARTESIAN_POINT ( 'NONE',  ( -10.00000000000000000, 1.224646799147353256E-15, 140.0000000000000000 ) ) ;
#2522 = DIRECTION ( 'NONE',  ( 1.000000000000000000, 1.734723475976806848E-16, 0.000000000000000000 ) ) ;
#2523 = ORIENTED_EDGE ( 'NONE', *, *, #3038, .T. ) ;
#2524 = EDGE_CURVE ( 'NONE', #4773, #7074, #883, .T. ) ;
#2525 = DIRECTION ( 'NONE',  ( -0.000000000000000000, 0.000000000000000000, -1.000000000000000000 ) ) ;
#2526 = DIRECTION ( 'NONE',  ( 0.000000000000000000, 0.000000000000000000, 1.000000000000000000 ) ) ;
#2527 = DIRECTION ( 'NONE',  ( 0.000000000000000000, 0.000000000000000000, 1.000000000000000000 ) ) ;
#2528 = ORIENTED_EDGE ( 'NONE', *, *, #2663, .F. ) ;
#2529 = ORIENTED_EDGE ( 'NONE', *, *, #8506, .T. ) ;
#2530 = ADVANCED_FACE ( 'NONE', ( #215 ), #2281, .F. ) ;
#2531 = DIRECTION ( 'NONE',  ( 0.000000000000000000, 0.000000000000000000, -1.000000000000000000 ) ) ;
#2532 = DIRECTION ( 'NONE',  ( -1.000000000000000000, 1.734723475976807341E-16, -0.000000000000000000 ) ) ;
#2533 = EDGE_CURVE ( 'NONE', #5002, #7356, #8200, .T. ) ;
#2534 = EDGE_CURVE ( 'NONE', #7663, #2610, #4846, .T. ) ;
#2535 = DIRECTION ( 'NONE',  ( 0.000000000000000000, 0.000000000000000000, 1.000000000000000000 ) ) ;
#2536 =( GEOMETRIC_REPRESENTATION_CONTEXT ( 3 ) GLOBAL_UNCERTAINTY_ASSIGNED_CONTEXT ( ( #7071 ) ) GLOBAL_UNIT_ASSIGNED_CONTEXT ( ( #743, #564, #4743 ) ) REPRESENTATION_CONTEXT ( 'NONE', 'WORKASPACE' ) );
#2537 = DIRECTION ( 'NONE',  ( 0.000000000000000000, 0.000000000000000000, -1.000000000000000000 ) ) ;
#2538 = ORIENTED_EDGE ( 'NONE', *, *, #4539, .F. ) ;
#2539 = ADVANCED_BREP_SHAPE_REPRESENTATION ( '', ( #4703, #594 ), #471 ) ;
#2540 = ORIENTED_EDGE ( 'NONE', *, *, #1410, .F. ) ;
#2541 = CARTESIAN_POINT ( 'NONE',  ( 3.453038570460273071, 2.625189405340834448, -3.535263753543585352 ) ) ;
#2542 = AXIS2_PLACEMENT_3D ( 'NONE', #7085, #383, #3088 ) ;
#2543=STYLED_ITEM('',(#8678),#4703);
#2544 = VECTOR ( 'NONE', #7857, 1000.000000000000000 ) ;
#2545 = FACE_BOUND ( 'NONE', #1409, .T. ) ;
#2546 = DIRECTION ( 'NONE',  ( 0.000000000000000000, 1.000000000000000000, 0.000000000000000000 ) ) ;
#2547 = DIRECTION ( 'NONE',  ( 1.000000000000000000, -1.734723475976806848E-16, 0.000000000000000000 ) ) ;
#2548 = CARTESIAN_POINT ( 'NONE',  ( 0.000000000000000000, -20.00000000000000000, -157.5000000000000284 ) ) ;
#2549 = AXIS2_PLACEMENT_3D ( 'NONE', #4576, #1402, #44 ) ;
#2550 = CARTESIAN_POINT ( 'NONE',  ( 0.000000000000000000, 0.000000000000000000, 0.000000000000000000 ) ) ;
#2551 = AXIS2_PLACEMENT_3D ( 'NONE', #4595, #7208, #5980 ) ;
#2552 = DIRECTION ( 'NONE',  ( 1.000000000000000000, 0.000000000000000000, 0.000000000000000000 ) ) ;
#2553 = DIRECTION ( 'NONE',  ( 0.000000000000000000, 1.000000000000000000, 0.000000000000000000 ) ) ;
#2554 = CIRCLE ( 'NONE', #3799, 10.00000000000000000 ) ;
#2555 = VECTOR ( 'NONE', #3733, 1000.000000000000000 ) ;
#2556 = DIRECTION ( 'NONE',  ( 0.000000000000000000, 1.000000000000000000, 0.000000000000000000 ) ) ;
#2557 = DIRECTION ( 'NONE',  ( -0.000000000000000000, -0.000000000000000000, -1.000000000000000000 ) ) ;
#2558 = ADVANCED_FACE ( 'NONE', ( #1579 ), #1489, .F. ) ;
#2559 = ORIENTED_EDGE ( 'NONE', *, *, #2265, .F. ) ;
#2560 = ADVANCED_FACE ( 'NONE', ( #1445 ), #7585, .F. ) ;
#2561 = PRESENTATION_STYLE_ASSIGNMENT (( #5841 ) ) ;
#2562 = DIRECTION ( 'NONE',  ( 0.000000000000000000, -0.000000000000000000, 1.000000000000000000 ) ) ;
#2563 = VERTEX_POINT ( 'NONE', #797 ) ;
#2564 = CARTESIAN_POINT ( 'NONE',  ( 0.000000000000000000, 0.000000000000000000, 0.000000000000000000 ) ) ;
#2565 = DIRECTION ( 'NONE',  ( -1.000000000000000000, 1.734723475976807587E-16, 0.000000000000000000 ) ) ;
#2566 = VECTOR ( 'NONE', #3629, 1000.000000000000000 ) ;
#2567 = CARTESIAN_POINT ( 'NONE',  ( 264.0000000000000000, -20.00000000000000000, -54.08142504031544462 ) ) ;
#2568 = ORIENTED_EDGE ( 'NONE', *, *, #4724, .T. ) ;
#2569 = CARTESIAN_POINT ( 'NONE',  ( 4.197393957002303999, 0.8151795401431359833, -3.503767560748935139 ) ) ;
#2570 = DIRECTION ( 'NONE',  ( -2.088802908413642958E-17, -1.000000000000000000, -8.060420609853009055E-17 ) ) ;
#2571 = PRODUCT_DEFINITION ( 'UNKNOWN', '', #1700, #2643 ) ;
#2572 = CARTESIAN_POINT ( 'NONE',  ( -0.6448876103708541807, -4.246476118072358474, -0.2256878752776773356 ) ) ;
#2573 = VERTEX_POINT ( 'NONE', #2231 ) ;
#2574 = ORIENTED_EDGE ( 'NONE', *, *, #2097, .F. ) ;
#2575 = CARTESIAN_POINT ( 'NONE',  ( 8.673617379884035472E-16, 4.618802153517012954, 0.000000000000000000 ) ) ;
#2576 = DIRECTION ( 'NONE',  ( -0.000000000000000000, -0.000000000000000000, 1.000000000000000000 ) ) ;
#2577 = CARTESIAN_POINT ( 'NONE',  ( 53.33333333333330017, -15.00000000000000000, 162.5000000000000853 ) ) ;
#2578 = CARTESIAN_POINT ( 'NONE',  ( -5.000000000000000000, -5.000000000000000000, 148.0000000000000284 ) ) ;
#2579 = ORIENTED_EDGE ( 'NONE', *, *, #4168, .T. ) ;
#2580 = EDGE_LOOP ( 'NONE', ( #5590, #6632, #2724, #1983 ) ) ;
#2581 = DIRECTION ( 'NONE',  ( -0.5000000000000051070, 0.000000000000000000, 0.8660254037844355990 ) ) ;
#2582 = CARTESIAN_POINT ( 'NONE',  ( 5.200000000000002842, 0.000000000000000000, 0.000000000000000000 ) ) ;
#2583 = CARTESIAN_POINT ( 'NONE',  ( 0.000000000000000000, 157.5000000000000284, 5.000000000000000888 ) ) ;
#2584 = CARTESIAN_POINT ( 'NONE',  ( -2.649999999999993694, 157.5000000000000284, 0.000000000000000000 ) ) ;
#2585 = APPLICATION_CONTEXT ( 'automotive_design' ) ;
#2586 =( NAMED_UNIT ( * ) PLANE_ANGLE_UNIT ( ) SI_UNIT ( $, .RADIAN. ) );
#2587 = EDGE_CURVE ( 'NONE', #1160, #5001, #4181, .T. ) ;
#2588 = CIRCLE ( 'NONE', #2171, 4.250000000000000000 ) ;
#2589 = DIRECTION ( 'NONE',  ( -0.000000000000000000, -0.000000000000000000, 1.000000000000000000 ) ) ;
#2590 = CARTESIAN_POINT ( 'NONE',  ( 4.000000000000000000, 0.000000000000000000, 0.000000000000000000 ) ) ;
#2591 = CARTESIAN_POINT ( 'NONE',  ( 5.000000000000001776, 134.9989999999999952, 15.00000000000000355 ) ) ;
#2592 = CIRCLE ( 'NONE', #1477, 10.00000000000000000 ) ;
#2593 = CARTESIAN_POINT ( 'NONE',  ( 176.0000000000000000, -20.00000000000000000, -89.28142504031545457 ) ) ;
#2594 = CARTESIAN_POINT ( 'NONE',  ( -5.000000000000000000, -5.000000000000000000, -97.99999999999997158 ) ) ;
#2595 = VECTOR ( 'NONE', #7384, 1000.000000000000000 ) ;
#2596 = EDGE_LOOP ( 'NONE', ( #1224, #385, #3516, #2405 ) ) ;
#2597 = PLANE ( 'NONE',  #4680 ) ;
#2598 = CONTEXT_DEPENDENT_SHAPE_REPRESENTATION ( #1815, #3103 ) ;
#2599 = ORIENTED_EDGE ( 'NONE', *, *, #6716, .T. ) ;
#2600 = DIRECTION ( 'NONE',  ( 0.000000000000000000, -1.224646799147353454E-16, 1.000000000000000000 ) ) ;
#2601 = DIRECTION ( 'NONE',  ( -0.000000000000000000, 1.000000000000000000, -0.000000000000000000 ) ) ;
#2602 = VECTOR ( 'NONE', #2291, 1000.000000000000000 ) ;
#2603 = EDGE_CURVE ( 'NONE', #3079, #2989, #2898, .T. ) ;
#2604 = AXIS2_PLACEMENT_3D ( 'NONE', #7359, #7319, #7403 ) ;
#2605 = DIRECTION ( 'NONE',  ( 0.000000000000000000, -1.000000000000000000, 0.000000000000000000 ) ) ;
#2606 = ORIENTED_EDGE ( 'NONE', *, *, #4298, .T. ) ;
#2607 = DIRECTION ( 'NONE',  ( -0.000000000000000000, -0.000000000000000000, 1.000000000000000000 ) ) ;
#2608 = DIRECTION ( 'NONE',  ( 0.3957342950827467121, -5.551115123125782702E-17, 0.9183650514339936066 ) ) ;
#2609 = FACE_BOUND ( 'NONE', #2257, .T. ) ;
#2610 = VERTEX_POINT ( 'NONE', #6921 ) ;
#2611 = ORIENTED_EDGE ( 'NONE', *, *, #627, .F. ) ;
#2612 = DIRECTION ( 'NONE',  ( 0.000000000000000000, 0.000000000000000000, -1.000000000000000000 ) ) ;
#2613 = CARTESIAN_POINT ( 'NONE',  ( 0.000000000000000000, 0.000000000000000000, -115.0000000000000000 ) ) ;
#2614 = PRODUCT_DEFINITION ( 'UNKNOWN', '', #13, #1951 ) ;
#2615 = CARTESIAN_POINT ( 'NONE',  ( 1.655952806101427033, -3.662737355149048302, -1.182683869819604841E-14 ) ) ;
#2616 = DIRECTION ( 'NONE',  ( 0.000000000000000000, 0.000000000000000000, -1.000000000000000000 ) ) ;
#2617 = ORIENTED_EDGE ( 'NONE', *, *, #3587, .F. ) ;
#2618 = ORIENTED_EDGE ( 'NONE', *, *, #282, .T. ) ;
#2619 = CARTESIAN_POINT ( 'NONE',  ( 5.000000000000001776, -4.999999999999998224, 140.0000000000000000 ) ) ;
#2620 = AXIS2_PLACEMENT_3D ( 'NONE', #7882, #1884, #7263 ) ;
#2621 = CARTESIAN_POINT ( 'NONE',  ( 53.33333333333330017, -20.00000000000000000, 162.5000000000000853 ) ) ;
#2622 = LINE ( 'NONE', #5354, #6511 ) ;
#2623 = ORIENTED_EDGE ( 'NONE', *, *, #1454, .T. ) ;
#2624 = CARTESIAN_POINT ( 'NONE',  ( -4.000000000000000000, 2.309401076758498483, -3.433295621305379353 ) ) ;
#2625 = AXIS2_PLACEMENT_3D ( 'NONE', #7416, #7992, #7456 ) ;
#2626 = DIRECTION ( 'NONE',  ( -1.000000000000000000, 0.000000000000000000, 0.000000000000000000 ) ) ;
#2627 = FACE_BOUND ( 'NONE', #3355, .T. ) ;
#2628 = EDGE_CURVE ( 'NONE', #3075, #5045, #2922, .T. ) ;
#2629 = DIRECTION ( 'NONE',  ( 0.000000000000000000, 0.000000000000000000, 1.000000000000000000 ) ) ;
#2630 = ADVANCED_FACE ( 'NONE', ( #925, #3618, #4795, #6790, #4840, #7493 ), #5568, .T. ) ;
#2631 = AXIS2_PLACEMENT_3D ( 'NONE', #3409, #85, #8076 ) ;
#2632 = LINE ( 'NONE', #4758, #3202 ) ;
#2633 = ADVANCED_FACE ( 'NONE', ( #7628 ), #2456, .T. ) ;
#2634 = DIRECTION ( 'NONE',  ( -1.000000000000000000, 0.000000000000000000, 0.000000000000000000 ) ) ;
#2635 = DIRECTION ( 'NONE',  ( 0.000000000000000000, 0.000000000000000000, 1.000000000000000000 ) ) ;
#2636 = ORIENTED_EDGE ( 'NONE', *, *, #7800, .F. ) ;
#2637 = SHAPE_REPRESENTATION_RELATIONSHIP ( 'NONE' , 'NONE' ,  #7993, #3452 ) ;
#2638 = VERTEX_POINT ( 'NONE', #4358 ) ;
#2639 = ORIENTED_EDGE ( 'NONE', *, *, #2210, .F. ) ;
#2640 = DIRECTION ( 'NONE',  ( 0.000000000000000000, 0.000000000000000000, 1.000000000000000000 ) ) ;
#2641 = AXIS2_PLACEMENT_3D ( 'NONE', #3709, #1055, #4361 ) ;
#2642 = DIRECTION ( 'NONE',  ( 1.000000000000000000, 0.000000000000000000, 0.000000000000000000 ) ) ;
#2643 = PRODUCT_DEFINITION_CONTEXT ( 'detailed design', #5240, 'design' ) ;
#2644 = FACE_OUTER_BOUND ( 'NONE', #4907, .T. ) ;
#2645 = CONICAL_SURFACE ( 'NONE', #7364, 2.041999999999999815, 1.047197551196591858 ) ;
#2646 = ORIENTED_EDGE ( 'NONE', *, *, #7644, .F. ) ;
#2647 = CARTESIAN_POINT ( 'NONE',  ( -20.00000000000000000, 135.0000000000000000, 40.00000000000000000 ) ) ;
#2648 = CIRCLE ( 'NONE', #275, 4.000000000000000000 ) ;
#2649 = DIRECTION ( 'NONE',  ( 0.000000000000000000, 0.000000000000000000, 1.000000000000000000 ) ) ;
#2650 = FACE_OUTER_BOUND ( 'NONE', #5636, .T. ) ;
#2651 = ORIENTED_EDGE ( 'NONE', *, *, #4741, .F. ) ;
#2652 = EDGE_LOOP ( 'NONE', ( #2850, #3633 ) ) ;
#2653 = DIRECTION ( 'NONE',  ( -0.000000000000000000, -0.000000000000000000, 1.000000000000000000 ) ) ;
#2654 = DIRECTION ( 'NONE',  ( 0.000000000000000000, -0.000000000000000000, -1.000000000000000000 ) ) ;
#2655 = CARTESIAN_POINT ( 'NONE',  ( 4.197310751797292738, 0.8178363989516252985, -3.502498386812444409 ) ) ;
#2656 = CARTESIAN_POINT ( 'NONE',  ( 0.000000000000000000, 0.000000000000000000, -4.000000000000000000 ) ) ;
#2657 = ORIENTED_EDGE ( 'NONE', *, *, #3036, .F. ) ;
#2658 = ADVANCED_FACE ( 'NONE', ( #8330 ), #1053, .F. ) ;
#2659 = PRESENTATION_STYLE_ASSIGNMENT (( #8544 ) ) ;
#2660 = ADVANCED_FACE ( 'NONE', ( #7721 ), #5137, .F. ) ;
#2661 = EDGE_LOOP ( 'NONE', ( #7288, #6976, #6325, #3445 ) ) ;
#2662 = DIRECTION ( 'NONE',  ( -1.000000000000000000, 0.000000000000000000, 0.000000000000000000 ) ) ;
#2663 = EDGE_CURVE ( 'NONE', #5369, #5286, #7802, .T. ) ;
#2664 = FACE_OUTER_BOUND ( 'NONE', #1690, .T. ) ;
#2665 = DIRECTION ( 'NONE',  ( -0.000000000000000000, -0.000000000000000000, 1.000000000000000000 ) ) ;
#2666 = EDGE_CURVE ( 'NONE', #6335, #1556, #8419, .T. ) ;
#2667 = ORIENTED_EDGE ( 'NONE', *, *, #1892, .F. ) ;
#2668 = DIRECTION ( 'NONE',  ( -0.000000000000000000, 1.000000000000000000, -0.000000000000000000 ) ) ;
#2669 = AXIS2_PLACEMENT_3D ( 'NONE', #339, #8321, #4999 ) ;
#2670 = PRODUCT_DEFINITION_SHAPE ( 'NONE', 'NONE',  #8602 ) ;
#2671 = ADVANCED_FACE ( 'NONE', ( #7141, #1008 ), #5093, .F. ) ;
#2672 = LINE ( 'NONE', #1092, #616 ) ;
#2673 = FACE_OUTER_BOUND ( 'NONE', #1394, .T. ) ;
#2674 = DIRECTION ( 'NONE',  ( -1.000000000000000000, 0.000000000000000000, 0.000000000000000000 ) ) ;
#2675 = AXIS2_PLACEMENT_3D ( 'NONE', #5143, #7807, #1843 ) ;
#2676 = DIRECTION ( 'NONE',  ( -0.000000000000000000, -0.000000000000000000, 1.000000000000000000 ) ) ;
#2677 = VERTEX_POINT ( 'NONE', #7675 ) ;
#2678 = CIRCLE ( 'NONE', #6695, 10.00000000000000000 ) ;
#2679 = ORIENTED_EDGE ( 'NONE', *, *, #6640, .F. ) ;
#2680 = UNCERTAINTY_MEASURE_WITH_UNIT (LENGTH_MEASURE( 1.000000000000000082E-05 ), #7558, 'distance_accuracy_value', 'NONE');
#2681 = ORIENTED_EDGE ( 'NONE', *, *, #577, .T. ) ;
#2682 = DIRECTION ( 'NONE',  ( -1.734723475976806848E-16, -1.000000000000000000, 0.000000000000000000 ) ) ;
#2683 = AXIS2_PLACEMENT_3D ( 'NONE', #1527, #8114, #792 ) ;
#2684 = ADVANCED_FACE ( 'NONE', ( #6355 ), #7761, .T. ) ;
#2685 = PLANE ( 'NONE',  #2278 ) ;
#2686 = VECTOR ( 'NONE', #5471, 1000.000000000000000 ) ;
#2687 = ORIENTED_EDGE ( 'NONE', *, *, #2256, .T. ) ;
#2688 = CARTESIAN_POINT ( 'NONE',  ( 53.33333333333330017, -20.00000000000000000, 165.1500000000000625 ) ) ;
#2689 = ORIENTED_EDGE ( 'NONE', *, *, #5886, .T. ) ;
#2690 = CARTESIAN_POINT ( 'NONE',  ( 0.000000000000000000, 0.000000000000000000, 120.0000000000000142 ) ) ;
#2691 = CARTESIAN_POINT ( 'NONE',  ( 82.99999999999998579, -4.999999999999998224, 139.9990000000000236 ) ) ;
#2692 = ADVANCED_FACE ( 'NONE', ( #1798 ), #3792, .T. ) ;
#2693 = CARTESIAN_POINT ( 'NONE',  ( 0.000000000000000000, -30.00000000000000355, -157.5000000000000284 ) ) ;
#2694 = DIRECTION ( 'NONE',  ( 0.000000000000000000, 0.000000000000000000, 1.000000000000000000 ) ) ;
#2695 = ORIENTED_EDGE ( 'NONE', *, *, #2851, .F. ) ;
#2696 = VECTOR ( 'NONE', #4418, 1000.000000000000000 ) ;
#2697 = VERTEX_POINT ( 'NONE', #1837 ) ;
#2698 =( GEOMETRIC_REPRESENTATION_CONTEXT ( 3 ) GLOBAL_UNCERTAINTY_ASSIGNED_CONTEXT ( ( #2074 ) ) GLOBAL_UNIT_ASSIGNED_CONTEXT ( ( #6421, #4250, #3288 ) ) REPRESENTATION_CONTEXT ( 'NONE', 'WORKASPACE' ) );
#2699 = FACE_BOUND ( 'NONE', #6652, .T. ) ;
#2700 = EDGE_CURVE ( 'NONE', #7614, #6221, #6646, .T. ) ;
#2701 = CARTESIAN_POINT ( 'NONE',  ( -20.00000000000000000, 2.449293598294706513E-15, 120.0000000000000142 ) ) ;
#2702 =( REPRESENTATION_RELATIONSHIP ('NONE','NONE', #3312, #4754 ) REPRESENTATION_RELATIONSHIP_WITH_TRANSFORMATION ( #3208 )SHAPE_REPRESENTATION_RELATIONSHIP( ) );
#2703 = VECTOR ( 'NONE', #5757, 1000.000000000000000 ) ;
#2704 = CARTESIAN_POINT ( 'NONE',  ( 4.000000000000000000, -2.471525695159793035, -3.686886880705770864 ) ) ;
#2705 = DIRECTION ( 'NONE',  ( -0.000000000000000000, -0.000000000000000000, 1.000000000000000000 ) ) ;
#2706 = ORIENTED_EDGE ( 'NONE', *, *, #7980, .F. ) ;
#2707 = SHAPE_REPRESENTATION ( 'base plate', ( #594 ), #6566 ) ;
#2708 = ORIENTED_EDGE ( 'NONE', *, *, #2378, .T. ) ;
#2709 = CARTESIAN_POINT ( 'NONE',  ( 88.00000000000000000, -25.00000000000000000, -121.8314250403154659 ) ) ;
#2710 = AXIS2_PLACEMENT_3D ( 'NONE', #7479, #822, #5516 ) ;
#2711 = ADVANCED_FACE ( 'NONE', ( #486 ), #3143, .T. ) ;
#2712 = ADVANCED_FACE ( 'NONE', ( #6487 ), #7093, .F. ) ;
#2713 = CARTESIAN_POINT ( 'NONE',  ( 434.9999999999999432, -4.999999999999998224, 139.9990000000000236 ) ) ;
#2714 = DIRECTION ( 'NONE',  ( 0.000000000000000000, 1.224646799147353207E-16, 1.000000000000000000 ) ) ;
#2715 = ORIENTED_EDGE ( 'NONE', *, *, #6850, .F. ) ;
#2716 = FACE_OUTER_BOUND ( 'NONE', #2447, .T. ) ;
#2717 = DIRECTION ( 'NONE',  ( -0.000000000000000000, -0.000000000000000000, 1.000000000000000000 ) ) ;
#2718 = DIRECTION ( 'NONE',  ( 1.734723475976806848E-16, -1.000000000000000000, -0.000000000000000000 ) ) ;
#2719 = CARTESIAN_POINT ( 'NONE',  ( 303.3333333333333144, -20.00000000000000000, 162.5000000000000853 ) ) ;
#2720 = ADVANCED_FACE ( 'NONE', ( #6963 ), #3183, .T. ) ;
#2721 = CARTESIAN_POINT ( 'NONE',  ( 5.000000000000000000, 5.000000000000000000, -63.99999999999997158 ) ) ;
#2722 = ORIENTED_EDGE ( 'NONE', *, *, #6366, .F. ) ;
#2723 = VECTOR ( 'NONE', #1170, 1000.000000000000000 ) ;
#2724 = ORIENTED_EDGE ( 'NONE', *, *, #1226, .T. ) ;
#2725 = EDGE_LOOP ( 'NONE', ( #3417, #3665, #3898, #6958 ) ) ;
#2726 = DIRECTION ( 'NONE',  ( 1.000000000000000000, 0.000000000000000000, 0.000000000000000000 ) ) ;
#2727 = FACE_OUTER_BOUND ( 'NONE', #5733, .T. ) ;
#2728 = VECTOR ( 'NONE', #6768, 1000.000000000000000 ) ;
#2729 = AXIS2_PLACEMENT_3D ( 'NONE', #1110, #3762, #4731 ) ;
#2730 = ORIENTED_EDGE ( 'NONE', *, *, #6736, .T. ) ;
#2731 = CARTESIAN_POINT ( 'NONE',  ( -30.00000000000002842, -20.00000000000000000, 140.0000000000000000 ) ) ;
#2732 = VERTEX_POINT ( 'NONE', #346 ) ;
#2733 = FACE_OUTER_BOUND ( 'NONE', #135, .T. ) ;
#2734 = DIRECTION ( 'NONE',  ( 0.000000000000000000, -1.000000000000000000, 0.000000000000000000 ) ) ;
#2735 = VERTEX_POINT ( 'NONE', #3014 ) ;
#2736 = ORIENTED_EDGE ( 'NONE', *, *, #6244, .T. ) ;
#2737 = VECTOR ( 'NONE', #891, 1000.000000000000000 ) ;
#2739 = AXIS2_PLACEMENT_3D ( 'NONE', #6572, #3274, #5263 ) ;
#2738 = CARTESIAN_POINT ( 'NONE',  ( 25.00000000000000000, 0.000000000000000000, 0.000000000000000000 ) ) ;
#2740 = DIRECTION ( 'NONE',  ( -1.000000000000000000, 0.000000000000000000, -0.000000000000000000 ) ) ;
#2741 = EDGE_CURVE ( 'NONE', #342, #8570, #7815, .T. ) ;
#2742 = EDGE_CURVE ( 'NONE', #6803, #7313, #108, .T. ) ;
#2743 = DIRECTION ( 'NONE',  ( -1.734723475976807587E-16, 1.000000000000000000, 0.000000000000000000 ) ) ;
#2744 = PRODUCT_DEFINITION_SHAPE ( 'NONE', 'NONE',  #8611 ) ;
#2745 = CARTESIAN_POINT ( 'NONE',  ( -4.197393957002303999, -7.773935952363655451E-14, -3.503767560748929810 ) ) ;
#2746 = ORIENTED_EDGE ( 'NONE', *, *, #6509, .F. ) ;
#2747 = EDGE_CURVE ( 'NONE', #8315, #3043, #5867, .T. ) ;
#2748 = DIRECTION ( 'NONE',  ( 1.000000000000000000, -1.734723475976806848E-16, 0.000000000000000000 ) ) ;
#2749 = ORIENTED_EDGE ( 'NONE', *, *, #4020, .T. ) ;
#2750 = ORIENTED_EDGE ( 'NONE', *, *, #551, .T. ) ;
#2751 = LINE ( 'NONE', #615, #6570 ) ;
#2752 =( REPRESENTATION_RELATIONSHIP ('NONE','NONE', #3312, #4754 ) REPRESENTATION_RELATIONSHIP_WITH_TRANSFORMATION ( #8312 )SHAPE_REPRESENTATION_RELATIONSHIP( ) );
#2753 = CARTESIAN_POINT ( 'NONE',  ( 0.000000000000000000, 0.000000000000000000, 120.0000000000000000 ) ) ;
#2754 = CIRCLE ( 'NONE', #3307, 2.500000000000001332 ) ;
#2755 = LINE ( 'NONE', #868, #6084 ) ;
#2756 = VERTEX_POINT ( 'NONE', #7219 ) ;
#2757 = CARTESIAN_POINT ( 'NONE',  ( 4.000000000000000000, -2.309401076758514915, -3.433295621305383349 ) ) ;
#2758 = ADVANCED_FACE ( 'NONE', ( #655 ), #1926, .F. ) ;
#2759 = LINE ( 'NONE', #6006, #449 ) ;
#2760 = CARTESIAN_POINT ( 'NONE',  ( 470.0000000000000000, -25.00000000000000000, 200.0000000000000000 ) ) ;
#2761 = DIRECTION ( 'NONE',  ( 1.000000000000000000, 0.000000000000000000, 0.000000000000000000 ) ) ;
#2762 = CARTESIAN_POINT ( 'NONE',  ( 0.000000000000000000, 0.000000000000000000, 140.0000000000000000 ) ) ;
#2763 = DIRECTION ( 'NONE',  ( 0.000000000000000000, 0.000000000000000000, 1.000000000000000000 ) ) ;
#2764 = VECTOR ( 'NONE', #1620, 1000.000000000000000 ) ;
#2765 = EDGE_LOOP ( 'NONE', ( #5019, #4745 ) ) ;
#2766 = ORIENTED_EDGE ( 'NONE', *, *, #704, .F. ) ;
#2767 = ORIENTED_EDGE ( 'NONE', *, *, #5228, .F. ) ;
#2768 = CARTESIAN_POINT ( 'NONE',  ( 0.000000000000000000, 0.000000000000000000, -115.0000000000000000 ) ) ;
#2769 = EDGE_CURVE ( 'NONE', #5441, #66, #7484, .T. ) ;
#2770 =( LENGTH_UNIT ( ) NAMED_UNIT ( * ) SI_UNIT ( .MILLI., .METRE. ) );
#2771 = VECTOR ( 'NONE', #7329, 1000.000000000000000 ) ;
#2772 = EDGE_LOOP ( 'NONE', ( #8362, #8413, #901, #8135, #6291 ) ) ;
#2773 = FACE_OUTER_BOUND ( 'NONE', #2353, .T. ) ;
#2774 = VERTEX_POINT ( 'NONE', #3266 ) ;
#2775 = FACE_OUTER_BOUND ( 'NONE', #3187, .T. ) ;
#2776 = CARTESIAN_POINT ( 'NONE',  ( -5.000000000000000000, -5.000000000000000000, 148.0000000000000284 ) ) ;
#2777 = AXIS2_PLACEMENT_3D ( 'NONE', #3153, #1192, #3849 ) ;
#2778 = APPLICATION_PROTOCOL_DEFINITION ( 'draft international standard', 'automotive_design', 1998, #9 ) ;
#2779 = EDGE_LOOP ( 'NONE', ( #7267, #8266, #284, #8531 ) ) ;
#2780 = ORIENTED_EDGE ( 'NONE', *, *, #4885, .T. ) ;
#2781 = CARTESIAN_POINT ( 'NONE',  ( -4.101948962585905356, -2.368261337751088824, -3.681124513963624167 ) ) ;
#2782 = LINE ( 'NONE', #2170, #1157 ) ;
#2783 = VECTOR ( 'NONE', #5536, 1000.000000000000000 ) ;
#2784 = FACE_BOUND ( 'NONE', #6488, .T. ) ;
#2785 = CYLINDRICAL_SURFACE ( 'NONE', #6793, 10.00000000000000000 ) ;
#2786 = ORIENTED_EDGE ( 'NONE', *, *, #3139, .F. ) ;
#2787 =( NAMED_UNIT ( * ) PLANE_ANGLE_UNIT ( ) SI_UNIT ( $, .RADIAN. ) );
#2788 = CARTESIAN_POINT ( 'NONE',  ( 20.00000000000000000, 175.0000000000000284, 5.000000000000000000 ) ) ;
#2789 = ORIENTED_EDGE ( 'NONE', *, *, #4020, .F. ) ;
#2790 = CARTESIAN_POINT ( 'NONE',  ( -2.345747346278108214, 3.264484291692489215, -0.01223254789873409049 ) ) ;
#2791 = EDGE_CURVE ( 'NONE', #104, #7983, #4561, .T. ) ;
#2792 = ADVANCED_FACE ( 'NONE', ( #4047 ), #535, .T. ) ;
#2793 = LINE ( 'NONE', #700, #7324 ) ;
#2794 = DIRECTION ( 'NONE',  ( 0.000000000000000000, 1.000000000000000000, 0.000000000000000000 ) ) ;
#2795 = EDGE_LOOP ( 'NONE', ( #4476, #3760, #7438, #3041 ) ) ;
#2796 = PLANE ( 'NONE',  #2631 ) ;
#2797 = DIRECTION ( 'NONE',  ( 1.000000000000000000, 0.000000000000000000, 0.000000000000000000 ) ) ;
#2798 = CARTESIAN_POINT ( 'NONE',  ( -5.000000000000000000, -5.000000000000000000, 148.0000000000000284 ) ) ;
#2799 = DIRECTION ( 'NONE',  ( 1.000000000000000000, 1.734723475976806848E-16, -0.000000000000000000 ) ) ;
#2800 = LINE ( 'NONE', #5366, #5127 ) ;
#2801 = DIRECTION ( 'NONE',  ( 0.8660254037844379305, 0.5000000000000013323, 0.000000000000000000 ) ) ;
#2802 = VECTOR ( 'NONE', #3586, 1000.000000000000000 ) ;
#2803 = VERTEX_POINT ( 'NONE', #1304 ) ;
#2804 = ORIENTED_EDGE ( 'NONE', *, *, #5409, .F. ) ;
#2805 = VERTEX_POINT ( 'NONE', #2578 ) ;
#2806 = FACE_OUTER_BOUND ( 'NONE', #6015, .T. ) ;
#2807 = DIRECTION ( 'NONE',  ( 0.000000000000000000, 0.000000000000000000, 1.000000000000000000 ) ) ;
#2808 = ADVANCED_FACE ( 'NONE', ( #562 ), #6604, .F. ) ;
#2809 = EDGE_CURVE ( 'NONE', #7561, #3699, #4604, .T. ) ;
#2810 = EDGE_CURVE ( 'NONE', #1077, #7459, #1364, .T. ) ;
#2811 = ORIENTED_EDGE ( 'NONE', *, *, #6878, .F. ) ;
#2812 = PLANE ( 'NONE',  #3422 ) ;
#2813 = VECTOR ( 'NONE', #931, 1000.000000000000000 ) ;
#2814 = ORIENTED_EDGE ( 'NONE', *, *, #4099, .F. ) ;
#2815 = CARTESIAN_POINT ( 'NONE',  ( 10.00000000000000000, 0.000000000000000000, -43.99999999999997158 ) ) ;
#2816 = FACE_OUTER_BOUND ( 'NONE', #7024, .T. ) ;
#2817 = CONTEXT_DEPENDENT_SHAPE_REPRESENTATION ( #8375, #4057 ) ;
#2818 = PLANE ( 'NONE',  #5169 ) ;
#2819 = EDGE_LOOP ( 'NONE', ( #1862, #22, #3504 ) ) ;
#2820 = AXIS2_PLACEMENT_3D ( 'NONE', #2420, #5055, #438 ) ;
#2821 = ORIENTED_EDGE ( 'NONE', *, *, #491, .T. ) ;
#2822 = CARTESIAN_POINT ( 'NONE',  ( 0.000000000000000000, 0.000000000000000000, 140.0000000000000000 ) ) ;
#2823 = LINE ( 'NONE', #8230, #3944 ) ;
#2824 = VECTOR ( 'NONE', #4081, 1000.000000000000000 ) ;
#2825 = CIRCLE ( 'NONE', #1987, 2.649999999999985700 ) ;
#2826 = VECTOR ( 'NONE', #7314, 1000.000000000000000 ) ;
#2827 = PLANE ( 'NONE',  #1059 ) ;
#2828 = CARTESIAN_POINT ( 'NONE',  ( 5.000000000000000000, 140.0000000000000000, 25.00000000000000000 ) ) ;
#2829 = EDGE_CURVE ( 'NONE', #8049, #997, #821, .T. ) ;
#2830 = ORIENTED_EDGE ( 'NONE', *, *, #4495, .F. ) ;
#2831 = DIRECTION ( 'NONE',  ( 0.000000000000000000, -1.000000000000000000, 0.000000000000000000 ) ) ;
#2832 =( GEOMETRIC_REPRESENTATION_CONTEXT ( 3 ) GLOBAL_UNCERTAINTY_ASSIGNED_CONTEXT ( ( #4675 ) ) GLOBAL_UNIT_ASSIGNED_CONTEXT ( ( #6248, #2478, #8350 ) ) REPRESENTATION_CONTEXT ( 'NONE', 'WORKASPACE' ) );
#2833 = CARTESIAN_POINT ( 'NONE',  ( -2.100000000000000089, 2.571758278209441957E-16, -0.2800830152838844622 ) ) ;
#2834 = ORIENTED_EDGE ( 'NONE', *, *, #2396, .F. ) ;
#2835 = CARTESIAN_POINT ( 'NONE',  ( 5.000000000000004441, 0.000000000000000000, 4.250000000000000000 ) ) ;
#2836 = FACE_BOUND ( 'NONE', #3650, .T. ) ;
#2837 = AXIS2_PLACEMENT_3D ( 'NONE', #6370, #7069, #2432 ) ;
#2838 = LINE ( 'NONE', #8198, #1774 ) ;
#2839 = LINE ( 'NONE', #4927, #8336 ) ;
#2840 = EDGE_LOOP ( 'NONE', ( #2121, #1707, #855, #7763 ) ) ;
#2841 = CARTESIAN_POINT ( 'NONE',  ( 0.000000000000000000, -20.00000000000000000, 0.000000000000000000 ) ) ;
#2842 = VECTOR ( 'NONE', #2125, 1000.000000000000000 ) ;
#2843 = DIRECTION ( 'NONE',  ( -0.000000000000000000, 0.000000000000000000, 1.000000000000000000 ) ) ;
#2844 = DIRECTION ( 'NONE',  ( -1.000000000000000000, 0.000000000000000000, 0.000000000000000000 ) ) ;
#2845 = ADVANCED_FACE ( 'NONE', ( #7309 ), #6691, .F. ) ;
#2846 = DIRECTION ( 'NONE',  ( -0.000000000000000000, 1.000000000000000000, -0.000000000000000000 ) ) ;
#2847 = EDGE_CURVE ( 'NONE', #2893, #2382, #4696, .T. ) ;
#2848 = CARTESIAN_POINT ( 'NONE',  ( -0.5636800770129166693, -4.293361309317430319, -3.531542292955206275 ) ) ;
#2849 = CARTESIAN_POINT ( 'NONE',  ( 444.9999999999999432, -4.999999999999998224, 145.0000000000000284 ) ) ;
#2850 = ORIENTED_EDGE ( 'NONE', *, *, #4226, .T. ) ;
#2851 = EDGE_CURVE ( 'NONE', #8533, #6097, #3353, .T. ) ;
#2852 = ORIENTED_EDGE ( 'NONE', *, *, #6007, .F. ) ;
#2853 = ORIENTED_EDGE ( 'NONE', *, *, #8476, .T. ) ;
#2854 = CARTESIAN_POINT ( 'NONE',  ( 2.500000000000000000, -1.178949249685213863, 2.042000000000002924 ) ) ;
#2855 = CARTESIAN_POINT ( 'NONE',  ( -4.999999999999998224, -4.999999999999998224, 140.0000000000000000 ) ) ;
#2856 = ORIENTED_EDGE ( 'NONE', *, *, #6529, .F. ) ;
#2857 = LINE ( 'NONE', #6202, #5911 ) ;
#2858 = ORIENTED_EDGE ( 'NONE', *, *, #3577, .F. ) ;
#2859 = CARTESIAN_POINT ( 'NONE',  ( 5.000000000000000888, 4.250000000000000000, 0.000000000000000000 ) ) ;
#2860 = APPLICATION_CONTEXT ( 'automotive_design' ) ;
#2861 = PLANE ( 'NONE',  #2873 ) ;
#2862 = CONTEXT_DEPENDENT_SHAPE_REPRESENTATION ( #3472, #7325 ) ;
#2863 = ORIENTED_EDGE ( 'NONE', *, *, #6242, .T. ) ;
#2864 = ORIENTED_EDGE ( 'NONE', *, *, #5439, .F. ) ;
#2865 = EDGE_CURVE ( 'NONE', #1248, #58, #7924, .T. ) ;
#2866 = CARTESIAN_POINT ( 'NONE',  ( -30.00000000000002842, -15.00000000000000000, 140.0000000000000000 ) ) ;
#2867 = CARTESIAN_POINT ( 'NONE',  ( -4.000000000000000000, 2.309401076758498483, -3.433295621305379353 ) ) ;
#2868 = VECTOR ( 'NONE', #4079, 1000.000000000000000 ) ;
#2869 = DIRECTION ( 'NONE',  ( -0.000000000000000000, -0.000000000000000000, 1.000000000000000000 ) ) ;
#2870 = CARTESIAN_POINT ( 'NONE',  ( 2.712762565639649015, -3.052587955997662306, -3.430618716626630871 ) ) ;
#2871 = ORIENTED_EDGE ( 'NONE', *, *, #6403, .T. ) ;
#2872 = AXIS2_PLACEMENT_3D ( 'NONE', #3414, #805, #6057 ) ;
#2873 = AXIS2_PLACEMENT_3D ( 'NONE', #1645, #4294, #7564 ) ;
#2874 = CARTESIAN_POINT ( 'NONE',  ( -4.203833317240879275, -1.627343821129593859, -3.597273115243890818 ) ) ;
#2875 = VERTEX_POINT ( 'NONE', #2055 ) ;
#2876 = CARTESIAN_POINT ( 'NONE',  ( -3.455068668934486276, 2.624017327439035707, -3.316620875263955437 ) ) ;
#2877 = DIRECTION ( 'NONE',  ( -0.000000000000000000, 1.000000000000000000, -0.000000000000000000 ) ) ;
#2878 = AXIS2_PLACEMENT_3D ( 'NONE', #4423, #1282, #8401 ) ;
#2879 = DIRECTION ( 'NONE',  ( 1.000000000000000000, 1.734723475976806848E-16, -0.000000000000000000 ) ) ;
#2880 = CARTESIAN_POINT ( 'NONE',  ( 259.0000000000000000, -4.999999999999998224, 139.9990000000000236 ) ) ;
#2881 = ORIENTED_EDGE ( 'NONE', *, *, #5342, .T. ) ;
#2882 = DIRECTION ( 'NONE',  ( 0.000000000000000000, 1.000000000000000000, 0.000000000000000000 ) ) ;
#2883 =( NAMED_UNIT ( * ) PLANE_ANGLE_UNIT ( ) SI_UNIT ( $, .RADIAN. ) );
#2884 = PRODUCT_DEFINITION_SHAPE ( 'NONE', 'NONE',  #8614 ) ;
#2885 = CARTESIAN_POINT ( 'NONE',  ( 0.000000000000000000, 0.000000000000000000, 120.0000000000000000 ) ) ;
#2886 = DIRECTION ( 'NONE',  ( -1.000000000000000000, 0.000000000000000000, 0.000000000000000000 ) ) ;
#2887 = LINE ( 'NONE', #6970, #2514 ) ;
#2888 = ADVANCED_FACE ( 'NONE', ( #7354, #1391 ), #6037, .F. ) ;
#2889 = PLANE ( 'NONE',  #4822 ) ;
#2890 = EDGE_LOOP ( 'NONE', ( #7846, #260, #766, #7376 ) ) ;
#2891 = ORIENTED_EDGE ( 'NONE', *, *, #6850, .T. ) ;
#2892 = EDGE_CURVE ( 'NONE', #3708, #2221, #4154, .T. ) ;
#2893 = VERTEX_POINT ( 'NONE', #2745 ) ;
#2894 = CARTESIAN_POINT ( 'NONE',  ( -5.000000000000000000, -5.000000000000000000, 140.0000000000000000 ) ) ;
#2895 = EDGE_CURVE ( 'NONE', #1258, #5075, #7893, .T. ) ;
#2896 = EDGE_CURVE ( 'NONE', #3043, #1905, #6822, .T. ) ;
#2897 = B_SPLINE_CURVE_WITH_KNOTS ( 'NONE', 3,
 ( #5670, #6144, #7685, #5015, #1586, #6848 ),
 .UNSPECIFIED., .F., .F.,
 ( 4, 2, 4 ),
 ( 0.002365888236227995517, 0.003551327329835084114, 0.004736766423442172712 ),
 .UNSPECIFIED. ) ;
#2898 = CIRCLE ( 'NONE', #7065, 20.00000000000000000 ) ;
#2899 = EDGE_LOOP ( 'NONE', ( #6308, #8395, #1794, #5554 ) ) ;
#2900 = LINE ( 'NONE', #8178, #7452 ) ;
#2901 = ORIENTED_EDGE ( 'NONE', *, *, #4626, .F. ) ;
#2902 = CARTESIAN_POINT ( 'NONE',  ( 303.3333333333333144, -20.00000000000000000, 162.5000000000000853 ) ) ;
#2903 = ITEM_DEFINED_TRANSFORMATION ( 'NONE', 'NONE', #3219,  #594 ) ;
#2904 = ORIENTED_EDGE ( 'NONE', *, *, #6192, .T. ) ;
#2905 = ORIENTED_EDGE ( 'NONE', *, *, #1392, .F. ) ;
#2906 = CARTESIAN_POINT ( 'NONE',  ( -20.00000000000000000, 175.0000000000000284, 5.000000000000000000 ) ) ;
#2907 = VECTOR ( 'NONE', #381, 1000.000000000000000 ) ;
#2908 = DIRECTION ( 'NONE',  ( -0.000000000000000000, -0.000000000000000000, -1.000000000000000000 ) ) ;
#2909 = DIRECTION ( 'NONE',  ( -0.000000000000000000, -0.000000000000000000, 1.000000000000000000 ) ) ;
#2910 = VECTOR ( 'NONE', #7322, 1000.000000000000000 ) ;
#2911 = CARTESIAN_POINT ( 'NONE',  ( 4.211140560182196957, 2.431303136016536470, -3.745885042887433514 ) ) ;
#2912 = ORIENTED_EDGE ( 'NONE', *, *, #7519, .F. ) ;
#2913 = CARTESIAN_POINT ( 'NONE',  ( 0.000000000000000000, 0.000000000000000000, 0.000000000000000000 ) ) ;
#2914 = CYLINDRICAL_SURFACE ( 'NONE', #3100, 2.649999999999985700 ) ;
#2915 = ORIENTED_EDGE ( 'NONE', *, *, #7146, .F. ) ;
#2916 = ORIENTED_EDGE ( 'NONE', *, *, #1226, .F. ) ;
#2917 = FACE_OUTER_BOUND ( 'NONE', #4200, .T. ) ;
#2918 = DIRECTION ( 'NONE',  ( -0.000000000000000000, -0.000000000000000000, -1.000000000000000000 ) ) ;
#2919 = CIRCLE ( 'NONE', #6805, 2.500000000000000444 ) ;
#2920 = DIRECTION ( 'NONE',  ( -0.000000000000000000, -0.000000000000000000, 1.000000000000000000 ) ) ;
#2921 = ADVANCED_FACE ( 'NONE', ( #4133 ), #247, .F. ) ;
#2922 = LINE ( 'NONE', #837, #8190 ) ;
#2923 = ORIENTED_EDGE ( 'NONE', *, *, #1488, .T. ) ;
#2924 = ADVANCED_FACE ( 'NONE', ( #4830 ), #2785, .T. ) ;
#2925 = FACE_OUTER_BOUND ( 'NONE', #4152, .T. ) ;
#2926 = VECTOR ( 'NONE', #2546, 1000.000000000000000 ) ;
#2927 = EDGE_CURVE ( 'NONE', #3444, #2174, #6780, .T. ) ;
#2928 = DIRECTION ( 'NONE',  ( 0.000000000000000000, 0.000000000000000000, 1.000000000000000000 ) ) ;
#2929 = CARTESIAN_POINT ( 'NONE',  ( -10.00000000000000000, 1.224646799147353256E-15, 62.00000000000001421 ) ) ;
#2930 = CARTESIAN_POINT ( 'NONE',  ( 470.0000000000000000, -20.00000000000000000, 140.0000000000000000 ) ) ;
#2931 = LINE ( 'NONE', #5147, #1107 ) ;
#2932 = SURFACE_SIDE_STYLE ('',( #8254 ) ) ;
#2934 = ORIENTED_EDGE ( 'NONE', *, *, #7331, .F. ) ;
#2933 = ADVANCED_FACE ( 'NONE', ( #6870 ), #8105, .T. ) ;
#2935 = ORIENTED_EDGE ( 'NONE', *, *, #8409, .F. ) ;
#2936 = ORIENTED_EDGE ( 'NONE', *, *, #841, .T. ) ;
#2937 = CARTESIAN_POINT ( 'NONE',  ( 5.000000000000000000, 5.000000000000000000, -105.9999999999999858 ) ) ;
#2938 = LINE ( 'NONE', #7775, #2286 ) ;
#2939 = VERTEX_POINT ( 'NONE', #6118 ) ;
#2940 = CARTESIAN_POINT ( 'NONE',  ( 0.2500000000000002220, 0.000000000000000000, 0.000000000000000000 ) ) ;
#2941 = EDGE_LOOP ( 'NONE', ( #527, #4676, #2736, #2084 ) ) ;
#2942 =( NAMED_UNIT ( * ) PLANE_ANGLE_UNIT ( ) SI_UNIT ( $, .RADIAN. ) );
#2943 = LINE ( 'NONE', #8351, #362 ) ;
#2944 = ORIENTED_EDGE ( 'NONE', *, *, #2791, .T. ) ;
#2945 = UNCERTAINTY_MEASURE_WITH_UNIT (LENGTH_MEASURE( 1.000000000000000082E-05 ), #2390, 'distance_accuracy_value', 'NONE');
#2946 = EDGE_CURVE ( 'NONE', #7213, #3247, #3466, .T. ) ;
#2947 = ORIENTED_EDGE ( 'NONE', *, *, #3116, .T. ) ;
#2948 = PRODUCT_DEFINITION_FORMATION_WITH_SPECIFIED_SOURCE ( 'ANY', '', #8104, .NOT_KNOWN. ) ;
#2949 = DIRECTION ( 'NONE',  ( -0.000000000000000000, 1.000000000000000000, -0.000000000000000000 ) ) ;
#2950 = FACE_OUTER_BOUND ( 'NONE', #1412, .T. ) ;
#2951 = VECTOR ( 'NONE', #5667, 1000.000000000000000 ) ;
#2952 = LINE ( 'NONE', #152, #7867 ) ;
#2953 = PRODUCT_DEFINITION_SHAPE ( 'NONE', 'NONE',  #8636 ) ;
#2954 = CARTESIAN_POINT ( 'NONE',  ( 0.000000000000000000, 0.000000000000000000, -63.99999999999997158 ) ) ;
#2955 = EDGE_CURVE ( 'NONE', #2563, #5355, #4432, .T. ) ;
#2956 = ORIENTED_EDGE ( 'NONE', *, *, #7731, .F. ) ;
#2957 =( LENGTH_UNIT ( ) NAMED_UNIT ( * ) SI_UNIT ( .MILLI., .METRE. ) );
#2958 = LINE ( 'NONE', #2404, #2518 ) ;
#2959 = EDGE_LOOP ( 'NONE', ( #3998, #1522, #3558, #8219 ) ) ;
#2960 = EDGE_CURVE ( 'NONE', #732, #3015, #4786, .T. ) ;
#2961 = EDGE_LOOP ( 'NONE', ( #7824, #6467 ) ) ;
#2962 = CONICAL_SURFACE ( 'NONE', #3106, 5.560781378645573980, 1.221730476396046816 ) ;
#2963 = DIRECTION ( 'NONE',  ( -1.734723475976806848E-16, -1.000000000000000000, 0.000000000000000000 ) ) ;
#2964 = CARTESIAN_POINT ( 'NONE',  ( 352.0000000000000000, -20.00000000000000000, -13.58142504031548192 ) ) ;
#2965 = CIRCLE ( 'NONE', #598, 10.00000000000000000 ) ;
#2966 = AXIS2_PLACEMENT_3D ( 'NONE', #5977, #7951, #7242 ) ;
#2967 = PRESENTATION_LAYER_ASSIGNMENT (  '', '', ( #7139 ) ) ;
#2968 = DIRECTION ( 'NONE',  ( -0.000000000000000000, 1.000000000000000000, -0.000000000000000000 ) ) ;
#2969 = CARTESIAN_POINT ( 'NONE',  ( 5.000000000000000000, -5.000000000000000000, -105.9999999999999858 ) ) ;
#2970 = ORIENTED_EDGE ( 'NONE', *, *, #8328, .F. ) ;
#2971 = FACE_BOUND ( 'NONE', #2477, .T. ) ;
#2972 = SURFACE_STYLE_FILL_AREA ( #6183 ) ;
#2973 = DIRECTION ( 'NONE',  ( -0.000000000000000000, 1.000000000000000000, -0.000000000000000000 ) ) ;
#2974 = VECTOR ( 'NONE', #2433, 1000.000000000000000 ) ;
#2975 = ADVANCED_FACE ( 'NONE', ( #2133 ), #7094, .F. ) ;
#2976 = DIRECTION ( 'NONE',  ( 0.000000000000000000, 0.000000000000000000, -1.000000000000000000 ) ) ;
#2977 = CIRCLE ( 'NONE', #612, 4.250000000000000000 ) ;
#2978 = LINE ( 'NONE', #7638, #7500 ) ;
#2979 = DIRECTION ( 'NONE',  ( 0.000000000000000000, 0.000000000000000000, 1.000000000000000000 ) ) ;
#2980 = DIRECTION ( 'NONE',  ( 1.000000000000000000, 0.000000000000000000, 0.000000000000000000 ) ) ;
#2981 = VECTOR ( 'NONE', #1750, 1000.000000000000000 ) ;
#2982 = ORIENTED_EDGE ( 'NONE', *, *, #8547, .T. ) ;
#2983 = VERTEX_POINT ( 'NONE', #4218 ) ;
#2984 = SHAPE_REPRESENTATION ( 'roller axis assy_r2', ( #594 ), #471 ) ;
#2985 = ORIENTED_EDGE ( 'NONE', *, *, #200, .F. ) ;
#2986 = CARTESIAN_POINT ( 'NONE',  ( -6.259644161404862988E-16, -4.618802153517027165, -3.504271511726793076 ) ) ;
#2987 = CARTESIAN_POINT ( 'NONE',  ( 53.33333333333330017, -14.99999999999999822, 165.1500000000000625 ) ) ;
#2988 = AXIS2_PLACEMENT_3D ( 'NONE', #8239, #2877, #298 ) ;
#2989 = VERTEX_POINT ( 'NONE', #8062 ) ;
#2990 = FILL_AREA_STYLE ('',( #8435 ) ) ;
#2991 = ORIENTED_EDGE ( 'NONE', *, *, #7865, .F. ) ;
#2992 = CYLINDRICAL_SURFACE ( 'NONE', #1768, 20.00000000000000000 ) ;
#2993 = CONTEXT_DEPENDENT_SHAPE_REPRESENTATION ( #1241, #8391 ) ;
#2994 = ORIENTED_EDGE ( 'NONE', *, *, #8204, .T. ) ;
#2995 = EDGE_LOOP ( 'NONE', ( #987, #5201, #2457, #3126 ) ) ;
#2996 = DIRECTION ( 'NONE',  ( -0.000000000000000000, -0.000000000000000000, 1.000000000000000000 ) ) ;
#2997 = PLANE ( 'NONE',  #6856 ) ;
#2998 = DIRECTION ( 'NONE',  ( -1.000000000000000000, 0.000000000000000000, 0.000000000000000000 ) ) ;
#2999 = CARTESIAN_POINT ( 'NONE',  ( 5.200000000000002842, 0.000000000000000000, -2.700000000000001066 ) ) ;
#3000 = EDGE_LOOP ( 'NONE', ( #6420, #5647, #2881, #746 ) ) ;
#3001 = CARTESIAN_POINT ( 'NONE',  ( 0.000000000000000000, -20.00000000000000000, 0.000000000000000000 ) ) ;
#3002 = CARTESIAN_POINT ( 'NONE',  ( 0.000000000000000000, 0.000000000000000000, 140.0000000000000000 ) ) ;
#3003 = EDGE_LOOP ( 'NONE', ( #5120, #2599, #2528, #4172 ) ) ;
#3004 = ORIENTED_EDGE ( 'NONE', *, *, #7979, .F. ) ;
#3005 = VECTOR ( 'NONE', #246, 1000.000000000000000 ) ;
#3006 = EDGE_CURVE ( 'NONE', #7579, #997, #2090, .T. ) ;
#3007 = CARTESIAN_POINT ( 'NONE',  ( 88.00000000000000000, -20.00000000000000000, -124.4814250403154574 ) ) ;
#3008 = CARTESIAN_POINT ( 'NONE',  ( 1.999999999999998224, -3.464101615137772594, -3.142992957459239012 ) ) ;
#3009 = EDGE_CURVE ( 'NONE', #7420, #1514, #4662, .T. ) ;
#3010 = EDGE_CURVE ( 'NONE', #3609, #1026, #7042, .T. ) ;
#3011 = CONICAL_SURFACE ( 'NONE', #3561, 2.500000000000000888, 0.9599310885968785900 ) ;
#3012 = FACE_OUTER_BOUND ( 'NONE', #7621, .T. ) ;
#3013 = AXIS2_PLACEMENT_3D ( 'NONE', #2043, #3429, #4687 ) ;
#3014 = CARTESIAN_POINT ( 'NONE',  ( 5.000000000000000000, 5.000000000000000000, 145.0000000000000284 ) ) ;
#3015 = VERTEX_POINT ( 'NONE', #7900 ) ;
#3016 = CARTESIAN_POINT ( 'NONE',  ( -31.74999999999995737, 0.000000000000000000, 0.000000000000000000 ) ) ;
#3017 = ORIENTED_EDGE ( 'NONE', *, *, #445, .T. ) ;
#3018 = FACE_OUTER_BOUND ( 'NONE', #3863, .T. ) ;
#3019 = VECTOR ( 'NONE', #673, 1000.000000000000000 ) ;
#3020 = CIRCLE ( 'NONE', #937, 2.649999999999985700 ) ;
#3021 = PLANE ( 'NONE',  #27 ) ;
#3022 = DIRECTION ( 'NONE',  ( 0.000000000000000000, 1.000000000000000000, 0.000000000000000000 ) ) ;
#3023 = CARTESIAN_POINT ( 'NONE',  ( 1.734723475976807094E-15, 4.618802153517012954, -0.4999999999999995559 ) ) ;
#3024 = CARTESIAN_POINT ( 'NONE',  ( -4.000000000000000000, 1.700094919196744270, -3.320312364301766017 ) ) ;
#3025 = EDGE_CURVE ( 'NONE', #6857, #8131, #5256, .T. ) ;
#3026 = ORIENTED_EDGE ( 'NONE', *, *, #2112, .F. ) ;
#3027 = EDGE_LOOP ( 'NONE', ( #4223, #3721, #5454, #4589 ) ) ;
#3028 = EDGE_LOOP ( 'NONE', ( #185, #4690, #2141, #1206 ) ) ;
#3029 = DIRECTION ( 'NONE',  ( 0.000000000000000000, 0.000000000000000000, 1.000000000000000000 ) ) ;
#3030 = AXIS2_PLACEMENT_3D ( 'NONE', #2583, #8591, #3975 ) ;
#3031 = DIRECTION ( 'NONE',  ( -0.000000000000000000, 1.000000000000000000, -0.000000000000000000 ) ) ;
#3032 =( REPRESENTATION_RELATIONSHIP ('NONE','NONE', #3312, #4754 ) REPRESENTATION_RELATIONSHIP_WITH_TRANSFORMATION ( #3514 )SHAPE_REPRESENTATION_RELATIONSHIP( ) );
#3033 = PRODUCT_DEFINITION_SHAPE ( 'NONE', 'NONE',  #8626 ) ;
#3034 = EDGE_LOOP ( 'NONE', ( #5617, #6860, #3842, #4962 ) ) ;
#3035 = CARTESIAN_POINT ( 'NONE',  ( 5.000000000000000000, 5.000000000000000000, -97.99999999999997158 ) ) ;
#3036 = EDGE_CURVE ( 'NONE', #5928, #5141, #4019, .T. ) ;
#3037 = ORIENTED_EDGE ( 'NONE', *, *, #7557, .T. ) ;
#3038 = EDGE_CURVE ( 'NONE', #7972, #6999, #3885, .T. ) ;
#3039 = PRESENTATION_STYLE_ASSIGNMENT (( #372 ) ) ;
#3040 = CARTESIAN_POINT ( 'NONE',  ( 0.000000000000000000, 0.000000000000000000, -135.0000000000000000 ) ) ;
#3041 = ORIENTED_EDGE ( 'NONE', *, *, #4660, .T. ) ;
#3042 = ADVANCED_FACE ( 'NONE', ( #6998 ), #4540, .F. ) ;
#3043 = VERTEX_POINT ( 'NONE', #7662 ) ;
#3044 = CARTESIAN_POINT ( 'NONE',  ( 136.6666666666666288, -25.00000000000000000, 165.1500000000000625 ) ) ;
#3045 = LINE ( 'NONE', #2445, #4771 ) ;
#3046 = DIRECTION ( 'NONE',  ( -1.000000000000000000, 0.000000000000000000, 0.000000000000000000 ) ) ;
#3047 = DIRECTION ( 'NONE',  ( -1.000000000000000000, 0.000000000000000000, 0.000000000000000000 ) ) ;
#3048 = ORIENTED_EDGE ( 'NONE', *, *, #363, .F. ) ;
#3049 = AXIS2_PLACEMENT_3D ( 'NONE', #6700, #662, #5956 ) ;
#3050 = CARTESIAN_POINT ( 'NONE',  ( 386.6666666666666288, -30.00000000000000355, 162.5000000000000853 ) ) ;
#3051 = FACE_OUTER_BOUND ( 'NONE', #2140, .T. ) ;
#3052 = ORIENTED_EDGE ( 'NONE', *, *, #5331, .F. ) ;
#3053 = ORIENTED_EDGE ( 'NONE', *, *, #3222, .T. ) ;
#3054 = CYLINDRICAL_SURFACE ( 'NONE', #5049, 2.649999999999985700 ) ;
#3055 = CYLINDRICAL_SURFACE ( 'NONE', #1309, 20.00000000000000000 ) ;
#3056 = EDGE_CURVE ( 'NONE', #6062, #3186, #7618, .T. ) ;
#3057 = AXIS2_PLACEMENT_3D ( 'NONE', #73, #5174, #4521 ) ;
#3058 = DIRECTION ( 'NONE',  ( -1.000000000000000000, 0.000000000000000000, 0.000000000000000000 ) ) ;
#3059 = DIRECTION ( 'NONE',  ( -1.000000000000000000, 0.000000000000000000, 0.000000000000000000 ) ) ;
#3060 = VERTEX_POINT ( 'NONE', #6501 ) ;
#3061 = EDGE_LOOP ( 'NONE', ( #2746, #2018, #2115, #2320 ) ) ;
#3062 = VECTOR ( 'NONE', #494, 1000.000000000000000 ) ;
#3063 = PLANE ( 'NONE',  #5587 ) ;
#3064 = EDGE_CURVE ( 'NONE', #6827, #5747, #3945, .T. ) ;
#3065 = PLANE ( 'NONE',  #8113 ) ;
#3066 = FACE_BOUND ( 'NONE', #3636, .T. ) ;
#3067 = CONICAL_SURFACE ( 'NONE', #6397, 2.041999999999999815, 1.047197551196591858 ) ;
#3068 = CARTESIAN_POINT ( 'NONE',  ( 259.0000000000000000, 5.000000000000001776, 140.0000000000000000 ) ) ;
#3069 = FACE_OUTER_BOUND ( 'NONE', #2941, .T. ) ;
#3070 = ORIENTED_EDGE ( 'NONE', *, *, #1374, .F. ) ;
#3071 = CARTESIAN_POINT ( 'NONE',  ( 3.680118525130245732, -2.494084732383344605, -0.3507732604232533524 ) ) ;
#3072 = FACE_BOUND ( 'NONE', #51, .T. ) ;
#3073 = CARTESIAN_POINT ( 'NONE',  ( 5.000000000000001776, -4.999999999999998224, 140.0000000000000000 ) ) ;
#3074 = UNCERTAINTY_MEASURE_WITH_UNIT (LENGTH_MEASURE( 1.000000000000000082E-05 ), #3269, 'distance_accuracy_value', 'NONE');
#3075 = VERTEX_POINT ( 'NONE', #1084 ) ;
#3076 = DIRECTION ( 'NONE',  ( 1.000000000000000000, 0.000000000000000000, 0.000000000000000000 ) ) ;
#3077 = ORIENTED_EDGE ( 'NONE', *, *, #3420, .T. ) ;
#3078 = CARTESIAN_POINT ( 'NONE',  ( -4.000000000000000000, 0.1981133338132459731, 2.096406544454392723E-17 ) ) ;
#3079 = VERTEX_POINT ( 'NONE', #5604 ) ;
#3080 = EDGE_LOOP ( 'NONE', ( #487, #7113 ) ) ;
#3081 = CARTESIAN_POINT ( 'NONE',  ( -5.000000000000000000, -5.000000000000000000, 140.0000000000000000 ) ) ;
#3082 = LINE ( 'NONE', #1741, #5874 ) ;
#3083 = ADVANCED_FACE ( 'NONE', ( #540 ), #3649, .F. ) ;
#3084 = EDGE_CURVE ( 'NONE', #1905, #8421, #582, .T. ) ;
#3085 = CARTESIAN_POINT ( 'NONE',  ( -4.000000000000000000, -0.7890432684750890990, -0.04868663549882315533 ) ) ;
#3086 = ORIENTED_EDGE ( 'NONE', *, *, #2847, .F. ) ;
#3087 = AXIS2_PLACEMENT_3D ( 'NONE', #2044, #4333, #4642 ) ;
#3088 = DIRECTION ( 'NONE',  ( 1.000000000000000000, 6.123233995736766036E-17, -6.123233995736764803E-17 ) ) ;
#3089 = PLANE ( 'NONE',  #1424 ) ;
#3090 = EDGE_LOOP ( 'NONE', ( #4873, #3990, #5523, #8304 ) ) ;
#3091 = AXIS2_PLACEMENT_3D ( 'NONE', #1335, #8140, #241 ) ;
#3092 = EDGE_LOOP ( 'NONE', ( #1711, #6658, #6786, #5840 ) ) ;
#3093 = CARTESIAN_POINT ( 'NONE',  ( 2.500000000000000000, -1.178949249685213863, 2.042000000000002924 ) ) ;
#3094 = CARTESIAN_POINT ( 'NONE',  ( 434.9999999999999432, 5.000000000000001776, 145.0000000000000284 ) ) ;
#3095 = CARTESIAN_POINT ( 'NONE',  ( 53.33333333333330017, -20.00000000000000000, 162.5000000000000853 ) ) ;
#3096 = CIRCLE ( 'NONE', #2549, 10.00000000000000000 ) ;
#3097 = CARTESIAN_POINT ( 'NONE',  ( 1.567478505476134606E-15, 4.618802153517012066, -3.433295621305382905 ) ) ;
#3098 = DIRECTION ( 'NONE',  ( -0.000000000000000000, -0.000000000000000000, 1.000000000000000000 ) ) ;
#3099 = ORIENTED_EDGE ( 'NONE', *, *, #8129, .T. ) ;
#3100 = AXIS2_PLACEMENT_3D ( 'NONE', #4175, #873, #3528 ) ;
#3101 = SURFACE_STYLE_USAGE ( .BOTH. , #1886 ) ;
#3102 = VERTEX_POINT ( 'NONE', #4390 ) ;
#3103 = PRODUCT_DEFINITION_SHAPE ( 'NONE', 'NONE',  #8629 ) ;
#3104 = CARTESIAN_POINT ( 'NONE',  ( 4.140404888673277384, 2.228338276487440428, -3.686887068327033390 ) ) ;
#3105 = VECTOR ( 'NONE', #5132, 1000.000000000000000 ) ;
#3106 = AXIS2_PLACEMENT_3D ( 'NONE', #4902, #1379, #4729 ) ;
#3107 = LINE ( 'NONE', #4410, #7881 ) ;
#3108 = LINE ( 'NONE', #4368, #693 ) ;
#3109 = VECTOR ( 'NONE', #555, 1000.000000000000000 ) ;
#3110 = CARTESIAN_POINT ( 'NONE',  ( -10.00000000000000000, 1.224646799147353256E-15, 27.00000000000000711 ) ) ;
#3111 = LINE ( 'NONE', #4935, #5919 ) ;
#3112 = EDGE_LOOP ( 'NONE', ( #2679, #8402, #5950, #4395, #3077 ) ) ;
#3113 = VECTOR ( 'NONE', #3560, 1000.000000000000000 ) ;
#3114 = SURFACE_SIDE_STYLE ('',( #3761 ) ) ;
#3115 = DIRECTION ( 'NONE',  ( 1.000000000000000000, 0.000000000000000000, 0.000000000000000000 ) ) ;
#3116 = EDGE_CURVE ( 'NONE', #1747, #6101, #5022, .T. ) ;
#3117 = DIRECTION ( 'NONE',  ( 0.000000000000000000, 0.000000000000000000, 1.000000000000000000 ) ) ;
#3118 = VECTOR ( 'NONE', #55, 1000.000000000000000 ) ;
#3119 = EDGE_CURVE ( 'NONE', #917, #5075, #1785, .T. ) ;
#3120 = ORIENTED_EDGE ( 'NONE', *, *, #7017, .F. ) ;
#3121 = PRESENTATION_STYLE_ASSIGNMENT (( #5635 ) ) ;
#3122 = ORIENTED_EDGE ( 'NONE', *, *, #5629, .F. ) ;
#3123 = CARTESIAN_POINT ( 'NONE',  ( 0.000000000000000000, 0.000000000000000000, 0.000000000000000000 ) ) ;
#3124 = DIRECTION ( 'NONE',  ( 1.000000000000000000, 1.734723475976806848E-16, -0.000000000000000000 ) ) ;
#3125 = CONTEXT_DEPENDENT_SHAPE_REPRESENTATION ( #3750, #5111 ) ;
#3126 = ORIENTED_EDGE ( 'NONE', *, *, #3802, .F. ) ;
#3127 = VERTEX_POINT ( 'NONE', #1235 ) ;
#3128 = AXIS2_PLACEMENT_3D ( 'NONE', #2613, #5254, #2740 ) ;
#3129 = DIRECTION ( 'NONE',  ( 1.734723475976807587E-16, 1.000000000000000000, 0.000000000000000000 ) ) ;
#3130 = LINE ( 'NONE', #333, #7133 ) ;
#3131 = DIRECTION ( 'NONE',  ( 1.000000000000000000, 0.000000000000000000, 0.000000000000000000 ) ) ;
#3132 = ORIENTED_EDGE ( 'NONE', *, *, #5250, .T. ) ;
#3133 = EDGE_CURVE ( 'NONE', #3710, #1611, #3324, .T. ) ;
#3134 = DIRECTION ( 'NONE',  ( 0.000000000000000000, 0.000000000000000000, 1.000000000000000000 ) ) ;
#3135 = CARTESIAN_POINT ( 'NONE',  ( 0.000000000000000000, 0.000000000000000000, -63.99999999999997158 ) ) ;
#3136 = ORIENTED_EDGE ( 'NONE', *, *, #8020, .F. ) ;
#3137 = EDGE_LOOP ( 'NONE', ( #7036, #7537 ) ) ;
#3138 = DIRECTION ( 'NONE',  ( 1.734723475976806848E-16, -1.000000000000000000, -0.000000000000000000 ) ) ;
#3139 = EDGE_CURVE ( 'NONE', #2080, #765, #6236, .T. ) ;
#3140 = FACE_OUTER_BOUND ( 'NONE', #5030, .T. ) ;
#3141 = B_SPLINE_CURVE_WITH_KNOTS ( 'NONE', 3,
 ( #1372, #5895, #718, #5159, #8564, #3952, #6674, #7164 ),
 .UNSPECIFIED., .F., .F.,
 ( 4, 2, 2, 4 ),
 ( 2.465131517075058656E-07, 0.001183067374689851080, 0.001774477805458923299, 0.002365888236227995517 ),
 .UNSPECIFIED. ) ;
#3142 = CARTESIAN_POINT ( 'NONE',  ( 4.000000000000000000, 2.309401076758497151, -3.433295621305379353 ) ) ;
#3143 = PLANE ( 'NONE',  #3182 ) ;
#3144 = VERTEX_POINT ( 'NONE', #1656 ) ;
#3145 = VECTOR ( 'NONE', #6388, 1000.000000000000000 ) ;
#3146 =( LENGTH_UNIT ( ) NAMED_UNIT ( * ) SI_UNIT ( .MILLI., .METRE. ) );
#3147 = ORIENTED_EDGE ( 'NONE', *, *, #7407, .T. ) ;
#3148 =( REPRESENTATION_RELATIONSHIP ('NONE','NONE', #3312, #4754 ) REPRESENTATION_RELATIONSHIP_WITH_TRANSFORMATION ( #4587 )SHAPE_REPRESENTATION_RELATIONSHIP( ) );
#3149 = DIRECTION ( 'NONE',  ( 1.000000000000000000, 0.000000000000000000, 0.000000000000000000 ) ) ;
#3150 = VECTOR ( 'NONE', #5506, 1000.000000000000000 ) ;
#3151 = DIRECTION ( 'NONE',  ( 1.000000000000000000, 0.000000000000000000, 0.000000000000000000 ) ) ;
#3152 = PLANE ( 'NONE',  #1536 ) ;
#3153 = CARTESIAN_POINT ( 'NONE',  ( 386.6666666666666288, -20.00000000000000000, 162.5000000000000853 ) ) ;
#3154 = CARTESIAN_POINT ( 'NONE',  ( 5.000000000000000000, 5.000000000000000000, -36.00000000000000000 ) ) ;
#3155=STYLED_ITEM('',(#8671),#1852);
#3156 = TOROIDAL_SURFACE ( 'NONE', #3436, 2.700000000000001066, 0.2000000000000000111 ) ;
#3157 = DIRECTION ( 'NONE',  ( -0.000000000000000000, -0.000000000000000000, 1.000000000000000000 ) ) ;
#3158 = DIRECTION ( 'NONE',  ( 0.000000000000000000, 1.000000000000000000, 0.000000000000000000 ) ) ;
#3159 = EDGE_CURVE ( 'NONE', #6262, #489, #5402, .T. ) ;
#3160 = CIRCLE ( 'NONE', #8451, 10.00000000000000000 ) ;
#3161 = VECTOR ( 'NONE', #2172, 1000.000000000000000 ) ;
#3162 = DIRECTION ( 'NONE',  ( 0.000000000000000000, 0.000000000000000000, 1.000000000000000000 ) ) ;
#3163 = EDGE_CURVE ( 'NONE', #6448, #5985, #2800, .T. ) ;
#3164 = ORIENTED_EDGE ( 'NONE', *, *, #1306, .T. ) ;
#3165 = PRODUCT_CONTEXT ( 'NONE', #7028, 'mechanical' ) ;
#3166 = DIRECTION ( 'NONE',  ( -1.000000000000000000, 0.000000000000000000, -0.000000000000000000 ) ) ;
#3167 = EDGE_CURVE ( 'NONE', #7751, #6101, #1981, .T. ) ;
#3168 = ORIENTED_EDGE ( 'NONE', *, *, #3357, .T. ) ;
#3169 = DIRECTION ( 'NONE',  ( -0.000000000000000000, -0.000000000000000000, -1.000000000000000000 ) ) ;
#3170 = EDGE_CURVE ( 'NONE', #5755, #6062, #1940, .T. ) ;
#3171 = FACE_BOUND ( 'NONE', #8408, .T. ) ;
#3172 = DIRECTION ( 'NONE',  ( 0.000000000000000000, 0.000000000000000000, 1.000000000000000000 ) ) ;
#3173 = ORIENTED_EDGE ( 'NONE', *, *, #627, .T. ) ;
#3174 = DIRECTION ( 'NONE',  ( 0.000000000000000000, 0.000000000000000000, 1.000000000000000000 ) ) ;
#3175 = DIRECTION ( 'NONE',  ( -0.06393308594707912407, -3.914772225553873302E-18, -0.9979541875864260669 ) ) ;
#3176 = CARTESIAN_POINT ( 'NONE',  ( -2.688821387764050996E-14, -4.618802153517012954, -0.4999999999999995559 ) ) ;
#3177 = VERTEX_POINT ( 'NONE', #1406 ) ;
#3178 = VERTEX_POINT ( 'NONE', #4716 ) ;
#3179 = FACE_OUTER_BOUND ( 'NONE', #1376, .T. ) ;
#3180 = FACE_OUTER_BOUND ( 'NONE', #5722, .T. ) ;
#3181 = DIRECTION ( 'NONE',  ( 0.000000000000000000, 0.000000000000000000, -1.000000000000000000 ) ) ;
#3182 = AXIS2_PLACEMENT_3D ( 'NONE', #3838, #3746, #4444 ) ;
#3183 = PLANE ( 'NONE',  #3595 ) ;
#3184 = VERTEX_POINT ( 'NONE', #672 ) ;
#3185 = FILL_AREA_STYLE_COLOUR ( '', #7411 ) ;
#3186 = VERTEX_POINT ( 'NONE', #3330 ) ;
#3187 = EDGE_LOOP ( 'NONE', ( #2574, #1648, #6032, #6934, #7249, #4325, #982 ) ) ;
#3188 = CARTESIAN_POINT ( 'NONE',  ( 2.836893136758676270, 3.208949435745843903, -3.505054077164911241 ) ) ;
#3189 = CIRCLE ( 'NONE', #5261, 2.100000000000000089 ) ;
#3190 = EDGE_CURVE ( 'NONE', #7290, #8085, #7286, .T. ) ;
#3191 = ADVANCED_FACE ( 'NONE', ( #3458 ), #6710, .T. ) ;
#3192 = FACE_OUTER_BOUND ( 'NONE', #3907, .T. ) ;
#3193 = CARTESIAN_POINT ( 'NONE',  ( -20.00000000000000000, 135.0000000000000000, 40.00000000000000000 ) ) ;
#3194 = EDGE_CURVE ( 'NONE', #1033, #4010, #1102, .T. ) ;
#3195 = DIRECTION ( 'NONE',  ( 0.000000000000000000, 0.000000000000000000, 1.000000000000000000 ) ) ;
#3196 =( REPRESENTATION_RELATIONSHIP ('NONE','NONE', #3312, #7424 ) REPRESENTATION_RELATIONSHIP_WITH_TRANSFORMATION ( #6423 )SHAPE_REPRESENTATION_RELATIONSHIP( ) );
#3197 = DIRECTION ( 'NONE',  ( 1.000000000000000000, 0.000000000000000000, 0.000000000000000000 ) ) ;
#3198 = VECTOR ( 'NONE', #3624, 1000.000000000000000 ) ;
#3199 = FACE_OUTER_BOUND ( 'NONE', #4594, .T. ) ;
#3200 = DIRECTION ( 'NONE',  ( -0.000000000000000000, -0.000000000000000000, 1.000000000000000000 ) ) ;
#3201 = CARTESIAN_POINT ( 'NONE',  ( 4.000000000000000000, 0.9868501483902631932, -0.09357334158579604100 ) ) ;
#3202 = VECTOR ( 'NONE', #4666, 1000.000000000000000 ) ;
#3203 = EDGE_CURVE ( 'NONE', #6725, #4773, #3189, .T. ) ;
#3204 = CARTESIAN_POINT ( 'NONE',  ( 0.000000000000000000, 0.000000000000000000, 120.0000000000000142 ) ) ;
#3205 = CARTESIAN_POINT ( 'NONE',  ( 25.00000000000000000, 0.000000000000000000, 0.000000000000000000 ) ) ;
#3206 = ORIENTED_EDGE ( 'NONE', *, *, #7605, .F. ) ;
#3207 = DIRECTION ( 'NONE',  ( -0.000000000000000000, 0.000000000000000000, -1.000000000000000000 ) ) ;
#3208 = ITEM_DEFINED_TRANSFORMATION ( 'NONE', 'NONE', #7243,  #594 ) ;
#3209 = VERTEX_POINT ( 'NONE', #1362 ) ;
#3210 = DIRECTION ( 'NONE',  ( 0.3713906763541037215, 0.000000000000000000, -0.9284766908852594147 ) ) ;
#3211 = DIRECTION ( 'NONE',  ( -0.000000000000000000, -0.000000000000000000, 1.000000000000000000 ) ) ;
#3212 = DIRECTION ( 'NONE',  ( -1.734723475976806848E-16, 1.000000000000000000, 0.000000000000000000 ) ) ;
#3213 = VERTEX_POINT ( 'NONE', #6095 ) ;
#3214 = LINE ( 'NONE', #8571, #5177 ) ;
#3215 = PRODUCT_CONTEXT ( 'NONE', #7764, 'mechanical' ) ;
#3216 = DIRECTION ( 'NONE',  ( 1.000000000000000000, 0.000000000000000000, 0.000000000000000000 ) ) ;
#3217 = ORIENTED_EDGE ( 'NONE', *, *, #5827, .T. ) ;
#3218 = ORIENTED_EDGE ( 'NONE', *, *, #2182, .T. ) ;
#3219 = AXIS2_PLACEMENT_3D ( 'NONE', #1480, #6121, #4347 ) ;
#3220 = CARTESIAN_POINT ( 'NONE',  ( -4.000000000000000000, -7.806255641895631925E-15, -3.142992957459232350 ) ) ;
#3221 = DIRECTION ( 'NONE',  ( -1.000000000000000000, 0.000000000000000000, 0.000000000000000000 ) ) ;
#3222 = EDGE_CURVE ( 'NONE', #1009, #1841, #130, .T. ) ;
#3223 = CARTESIAN_POINT ( 'NONE',  ( 181.0000000000000000, -4.999999999999998224, 145.0000000000000284 ) ) ;
#3224 = EDGE_CURVE ( 'NONE', #6827, #4339, #3388, .T. ) ;
#3225 = PRODUCT_DEFINITION_SHAPE ( 'NONE', 'NONE',  #6591 ) ;
#3226 = DIRECTION ( 'NONE',  ( -1.000000000000000000, -0.000000000000000000, -0.000000000000000000 ) ) ;
#3227 = ORIENTED_EDGE ( 'NONE', *, *, #6043, .T. ) ;
#3228 = EDGE_CURVE ( 'NONE', #7056, #5804, #8125, .T. ) ;
#3229 = SURFACE_SIDE_STYLE ('',( #8586 ) ) ;
#3230 = EDGE_LOOP ( 'NONE', ( #4334, #6713, #2519, #1534 ) ) ;
#3231 = DIRECTION ( 'NONE',  ( -1.000000000000000000, 0.000000000000000000, 0.000000000000000000 ) ) ;
#3232 = AXIS2_PLACEMENT_3D ( 'NONE', #4306, #6955, #998 ) ;
#3233 = AXIS2_PLACEMENT_3D ( 'NONE', #1215, #3873, #3260 ) ;
#3234 = VECTOR ( 'NONE', #3894, 1000.000000000000000 ) ;
#3235 = CARTESIAN_POINT ( 'NONE',  ( 4.211140560182196957, -2.431303136016555122, -3.745885042887436622 ) ) ;
#3236 = CARTESIAN_POINT ( 'NONE',  ( 439.9999999999999432, -25.00000000000000000, 16.31857495968447225 ) ) ;
#3237 = CARTESIAN_POINT ( 'NONE',  ( -20.00000000000000000, 140.0000000000000000, 40.00000000000000000 ) ) ;
#3238 = CIRCLE ( 'NONE', #592, 2.649999999999985700 ) ;
#3239 = EDGE_CURVE ( 'NONE', #5928, #7699, #4760, .T. ) ;
#3240 = CARTESIAN_POINT ( 'NONE',  ( 2.500000000000000000, 2.357898499370433054, -1.951563910473907981E-15 ) ) ;
#3241 = AXIS2_PLACEMENT_3D ( 'NONE', #7831, #6550, #685 ) ;
#3242 = LINE ( 'NONE', #5881, #3396 ) ;
#3243 = CARTESIAN_POINT ( 'NONE',  ( 4.211140560182196957, -2.431303136016555122, -3.745885042887436622 ) ) ;
#3244 = VECTOR ( 'NONE', #379, 1000.000000000000000 ) ;
#3245 = DIRECTION ( 'NONE',  ( 0.000000000000000000, -1.000000000000000000, 0.000000000000000000 ) ) ;
#3246 = LINE ( 'NONE', #7959, #647 ) ;
#3247 = VERTEX_POINT ( 'NONE', #4802 ) ;
#3248 = CARTESIAN_POINT ( 'NONE',  ( -4.000000000000000000, 0.3987449864459974846, -0.01220643443059782861 ) ) ;
#3249 = CONTEXT_DEPENDENT_SHAPE_REPRESENTATION ( #4082, #2344 ) ;
#3250 = ORIENTED_EDGE ( 'NONE', *, *, #200, .T. ) ;
#3251 = CARTESIAN_POINT ( 'NONE',  ( -20.00000000000000000, 2.449293598294706513E-15, -7.999999999999992895 ) ) ;
#3252 = LINE ( 'NONE', #4509, #1437 ) ;
#3253 = AXIS2_PLACEMENT_3D ( 'NONE', #1770, #622, #6581 ) ;
#3254 = PRODUCT_DEFINITION_CONTEXT ( 'detailed design', #8095, 'design' ) ;
#3255 = CARTESIAN_POINT ( 'NONE',  ( 0.000000000000000000, 0.000000000000000000, -7.999999999999996447 ) ) ;
#3256 = EDGE_LOOP ( 'NONE', ( #7714, #4397, #585, #7095 ) ) ;
#3257 = DIRECTION ( 'NONE',  ( 1.000000000000000000, 0.000000000000000000, 0.000000000000000000 ) ) ;
#3258 = AXIS2_PLACEMENT_3D ( 'NONE', #8368, #3743, #3835 ) ;
#3259 = PRODUCT_CONTEXT ( 'NONE', #6576, 'mechanical' ) ;
#3260 = DIRECTION ( 'NONE',  ( 0.000000000000000000, 0.000000000000000000, 1.000000000000000000 ) ) ;
#3261 = ORIENTED_EDGE ( 'NONE', *, *, #7524, .T. ) ;
#3262 = VERTEX_POINT ( 'NONE', #49 ) ;
#3263 = LINE ( 'NONE', #3964, #5457 ) ;
#3264 = DIRECTION ( 'NONE',  ( 0.000000000000000000, 1.000000000000000000, 0.000000000000000000 ) ) ;
#3265 = PLANE ( 'NONE',  #7734 ) ;
#3266 = CARTESIAN_POINT ( 'NONE',  ( 444.9999999999999432, -4.999999999999998224, 145.0000000000000284 ) ) ;
#3267 = ORIENTED_EDGE ( 'NONE', *, *, #830, .F. ) ;
#3268 = ADVANCED_FACE ( 'NONE', ( #6626 ), #5321, .F. ) ;
#3269 =( LENGTH_UNIT ( ) NAMED_UNIT ( * ) SI_UNIT ( .MILLI., .METRE. ) );
#3270 = VERTEX_POINT ( 'NONE', #4025 ) ;
#3271 = DIRECTION ( 'NONE',  ( 0.000000000000000000, 0.000000000000000000, -1.000000000000000000 ) ) ;
#3272 = EDGE_CURVE ( 'NONE', #7609, #5626, #4300, .T. ) ;
#3273 = ADVANCED_FACE ( 'NONE', ( #1498 ), #3413, .F. ) ;
#3274 = DIRECTION ( 'NONE',  ( -0.000000000000000000, 1.000000000000000000, -0.000000000000000000 ) ) ;
#3275 = DIRECTION ( 'NONE',  ( 0.000000000000000000, -1.000000000000000000, 0.000000000000000000 ) ) ;
#3276 = ORIENTED_EDGE ( 'NONE', *, *, #1410, .T. ) ;
#3277 = CARTESIAN_POINT ( 'NONE',  ( 2.500000000000000000, -1.768423874527823791, -1.020999999999998353 ) ) ;
#3278 = DIRECTION ( 'NONE',  ( -1.734723475976806848E-16, -1.000000000000000000, 0.000000000000000000 ) ) ;
#3279 = CIRCLE ( 'NONE', #4526, 2.649999999999985700 ) ;
#3280 = DIRECTION ( 'NONE',  ( 1.000000000000000000, -1.734723475976806848E-16, 0.000000000000000000 ) ) ;
#3281 = DIRECTION ( 'NONE',  ( -0.000000000000000000, -0.000000000000000000, 1.000000000000000000 ) ) ;
#3282 = EDGE_CURVE ( 'NONE', #479, #7567, #625, .T. ) ;
#3283 = PLANE ( 'NONE',  #1674 ) ;
#3284 = AXIS2_PLACEMENT_3D ( 'NONE', #2347, #461, #3634 ) ;
#3285 = CARTESIAN_POINT ( 'NONE',  ( -20.00000000000000000, 2.449293598294706513E-15, 62.00000000000001421 ) ) ;
#3286 = PLANE ( 'NONE',  #793 ) ;
#3287 = ORIENTED_EDGE ( 'NONE', *, *, #7271, .T. ) ;
#3288 =( NAMED_UNIT ( * ) SI_UNIT ( $, .STERADIAN. ) SOLID_ANGLE_UNIT ( ) );
#3289 = ORIENTED_EDGE ( 'NONE', *, *, #8388, .F. ) ;
#3290 = VERTEX_POINT ( 'NONE', #3285 ) ;
#3291 = DIRECTION ( 'NONE',  ( -0.000000000000000000, 1.000000000000000000, -0.000000000000000000 ) ) ;
#3292 = LINE ( 'NONE', #8520, #4355 ) ;
#3293=STYLED_ITEM('',(#8678),#1986);
#3294 = VECTOR ( 'NONE', #3317, 1000.000000000000000 ) ;
#3295 = EDGE_CURVE ( 'NONE', #6851, #7063, #6515, .T. ) ;
#3296 = EDGE_CURVE ( 'NONE', #6268, #8480, #1234, .T. ) ;
#3297 = DIRECTION ( 'NONE',  ( -0.000000000000000000, -0.000000000000000000, 1.000000000000000000 ) ) ;
#3298 = VERTEX_POINT ( 'NONE', #8339 ) ;
#3299 = LINE ( 'NONE', #2647, #5046 ) ;
#3300 = EDGE_CURVE ( 'NONE', #4379, #7751, #6090, .T. ) ;
#3301 = CARTESIAN_POINT ( 'NONE',  ( 88.00000000000000000, -30.00000000000000000, -121.8314250403154659 ) ) ;
#3302 = CARTESIAN_POINT ( 'NONE',  ( -2.000000000000007550, -3.464101615137749945, 0.000000000000000000 ) ) ;
#3303 = ORIENTED_EDGE ( 'NONE', *, *, #7658, .F. ) ;
#3304 = EDGE_LOOP ( 'NONE', ( #1436, #4905, #698, #5868, #375, #7779 ) ) ;
#3305 = LINE ( 'NONE', #1920, #314 ) ;
#3306 = PLANE ( 'NONE',  #3128 ) ;
#3307 = AXIS2_PLACEMENT_3D ( 'NONE', #829, #5479, #4832 ) ;
#3308 =( REPRESENTATION_RELATIONSHIP ('NONE','NONE', #3312, #872 ) REPRESENTATION_RELATIONSHIP_WITH_TRANSFORMATION ( #5074 )SHAPE_REPRESENTATION_RELATIONSHIP( ) );
#3309 = CARTESIAN_POINT ( 'NONE',  ( 5.000000000000004441, 0.000000000000000000, 0.000000000000000000 ) ) ;
#3310 = CARTESIAN_POINT ( 'NONE',  ( 386.6666666666666288, -20.00000000000000000, 162.5000000000000853 ) ) ;
#3311 = ORIENTED_EDGE ( 'NONE', *, *, #5228, .T. ) ;
#3312 = SHAPE_REPRESENTATION ( 'MAS-188', ( #2113, #6962, #138, #3219, #8089, #568, #5432, #5018, #1262, #1845, #6833, #2542, #5717, #3919, #4891, #5853, #6972, #2669, #2258, #148, #4471, #7534, #5298, #5165, #3232, #6416, #6689, #1415, #7952, #1142, #5989, #8240, #7243, #8510, #1558, #3087, #6278 ), #8377 ) ;
#3313 = APPLICATION_PROTOCOL_DEFINITION ( 'draft international standard', 'automotive_design', 1998, #5240 ) ;
#3314 = ORIENTED_EDGE ( 'NONE', *, *, #1263, .T. ) ;
#3315 = DIRECTION ( 'NONE',  ( 1.000000000000000000, 0.000000000000000000, 0.000000000000000000 ) ) ;
#3316 = AXIS2_PLACEMENT_3D ( 'NONE', #2880, #4103, #259 ) ;
#3317 = DIRECTION ( 'NONE',  ( 1.000000000000000000, 0.000000000000000000, 0.000000000000000000 ) ) ;
#3318 = CARTESIAN_POINT ( 'NONE',  ( 5.200000000000002842, 3.306546357697854719E-16, 2.700000000000001066 ) ) ;
#3319 = ORIENTED_EDGE ( 'NONE', *, *, #2810, .T. ) ;
#3320 = CARTESIAN_POINT ( 'NONE',  ( 5.000000000000000000, -5.000000000000000000, 148.0000000000000284 ) ) ;
#3321 = FACE_OUTER_BOUND ( 'NONE', #419, .T. ) ;
#3322 = UNCERTAINTY_MEASURE_WITH_UNIT (LENGTH_MEASURE( 1.000000000000000082E-05 ), #4689, 'distance_accuracy_value', 'NONE');
#3323 = EDGE_CURVE ( 'NONE', #186, #8517, #4849, .T. ) ;
#3324 = CIRCLE ( 'NONE', #257, 2.649999999999985700 ) ;
#3325 =( LENGTH_UNIT ( ) NAMED_UNIT ( * ) SI_UNIT ( .MILLI., .METRE. ) );
#3326 = CARTESIAN_POINT ( 'NONE',  ( 219.9999999999999716, -14.99999999999999822, 165.1500000000000625 ) ) ;
#3327 = CARTESIAN_POINT ( 'NONE',  ( -5.000000000000000000, -5.000000000000000000, -27.99999999999999645 ) ) ;
#3328 = CARTESIAN_POINT ( 'NONE',  ( 0.000000000000000000, 0.000000000000000000, -7.999999999999996447 ) ) ;
#3329 = EDGE_CURVE ( 'NONE', #4775, #5858, #2897, .T. ) ;
#3330 = CARTESIAN_POINT ( 'NONE',  ( 303.3333333333333144, -14.99999999999999822, 165.1500000000000625 ) ) ;
#3331 = CARTESIAN_POINT ( 'NONE',  ( 5.000000000000000000, -5.000000000000000000, 148.0000000000000284 ) ) ;
#3332 = ORIENTED_EDGE ( 'NONE', *, *, #7523, .F. ) ;
#3333 = ORIENTED_EDGE ( 'NONE', *, *, #6034, .F. ) ;
#3334 = B_SPLINE_CURVE_WITH_KNOTS ( 'NONE', 3,
 ( #2590, #6582, #579, #5233, #3201, #6536, #5317, #6460 ),
 .UNSPECIFIED., .F., .F.,
 ( 4, 2, 2, 4 ),
 ( 0.005725059856848645212, 0.006314084072593634418, 0.006903108288338624492, 0.008081156719828603771 ),
 .UNSPECIFIED. ) ;
#3335 = EDGE_LOOP ( 'NONE', ( #4009, #4834, #1670, #7132 ) ) ;
#3336 = LINE ( 'NONE', #3822, #7226 ) ;
#3337 = AXIS2_PLACEMENT_3D ( 'NONE', #1850, #493, #5708 ) ;
#3338 = LINE ( 'NONE', #4635, #7550 ) ;
#3339 = CARTESIAN_POINT ( 'NONE',  ( 2.500000000000000000, -2.357898499370432610, 3.252606517456513302E-15 ) ) ;
#3340 = CIRCLE ( 'NONE', #4450, 10.00000000000000000 ) ;
#3341 = EDGE_LOOP ( 'NONE', ( #5683, #3122, #1063, #7198 ) ) ;
#3342 = DIRECTION ( 'NONE',  ( -1.000000000000000000, 0.000000000000000000, 0.000000000000000000 ) ) ;
#3343 = DIRECTION ( 'NONE',  ( 0.000000000000000000, 1.000000000000000000, 0.000000000000000000 ) ) ;
#3344 =( NAMED_UNIT ( * ) SI_UNIT ( $, .STERADIAN. ) SOLID_ANGLE_UNIT ( ) );
#3345 = DIRECTION ( 'NONE',  ( 0.000000000000000000, 0.000000000000000000, 1.000000000000000000 ) ) ;
#3346 = ORIENTED_EDGE ( 'NONE', *, *, #7790, .F. ) ;
#3347 = VERTEX_POINT ( 'NONE', #4147 ) ;
#3348 = EDGE_CURVE ( 'NONE', #2875, #4853, #2290, .T. ) ;
#3349 = DIRECTION ( 'NONE',  ( 0.000000000000000000, -0.5000000000000012212, -0.8660254037844380415 ) ) ;
#3350 = ADVANCED_FACE ( 'NONE', ( #4188 ), #5035, .F. ) ;
#3351 = CARTESIAN_POINT ( 'NONE',  ( -20.00000000000000000, 2.449293598294706513E-15, 120.0000000000000142 ) ) ;
#3352 = CARTESIAN_POINT ( 'NONE',  ( -5.000000000000001776, 5.000000000000001776, 7.000000000000006217 ) ) ;
#3353 = LINE ( 'NONE', #5991, #7642 ) ;
#3354 = EDGE_LOOP ( 'NONE', ( #2864, #4104, #5130, #6098 ) ) ;
#3355 = EDGE_LOOP ( 'NONE', ( #7819, #894 ) ) ;
#3356 = LINE ( 'NONE', #8546, #4619 ) ;
#3357 = EDGE_CURVE ( 'NONE', #8365, #7520, #6655, .T. ) ;
#3358 = PLANE ( 'NONE',  #7606 ) ;
#3359 = CARTESIAN_POINT ( 'NONE',  ( 269.0000000000000000, -4.999999999999998224, 140.0000000000000000 ) ) ;
#3360 = EDGE_LOOP ( 'NONE', ( #1171, #2956, #2204, #3319 ) ) ;
#3361 = CARTESIAN_POINT ( 'NONE',  ( 2.500000000000000000, 2.357898499370433054, -1.951563910473907981E-15 ) ) ;
#3362 = PRODUCT_DEFINITION_FORMATION_WITH_SPECIFIED_SOURCE ( 'ANY', '', #1494, .NOT_KNOWN. ) ;
#3363 = PRODUCT_DEFINITION_SHAPE ( 'NONE', 'NONE',  #8609 ) ;
#3364 = CARTESIAN_POINT ( 'NONE',  ( 264.0000000000000000, -20.00000000000000000, -51.43142504031546025 ) ) ;
#3365 = CARTESIAN_POINT ( 'NONE',  ( 5.200000000000002842, 0.000000000000000000, 0.000000000000000000 ) ) ;
#3366 = AXIS2_PLACEMENT_3D ( 'NONE', #4799, #7453, #5492 ) ;
#3367 = DIRECTION ( 'NONE',  ( -0.000000000000000000, 1.000000000000000000, -0.000000000000000000 ) ) ;
#3368 = AXIS2_PLACEMENT_3D ( 'NONE', #6609, #4567, #3231 ) ;
#3369 = DIRECTION ( 'NONE',  ( -1.734723475976806848E-16, -1.000000000000000000, 0.000000000000000000 ) ) ;
#3370 = FACE_OUTER_BOUND ( 'NONE', #4211, .T. ) ;
#3371 = VERTEX_POINT ( 'NONE', #6890 ) ;
#3372 =( NAMED_UNIT ( * ) SI_UNIT ( $, .STERADIAN. ) SOLID_ANGLE_UNIT ( ) );
#3373 = CIRCLE ( 'NONE', #312, 2.499999999999999556 ) ;
#3374 = VERTEX_POINT ( 'NONE', #356 ) ;
#3375 = EDGE_CURVE ( 'NONE', #6933, #7290, #1542, .T. ) ;
#3376 = UNCERTAINTY_MEASURE_WITH_UNIT (LENGTH_MEASURE( 1.000000000000000082E-05 ), #1161, 'distance_accuracy_value', 'NONE');
#3377 = ORIENTED_EDGE ( 'NONE', *, *, #7932, .F. ) ;
#3378 = FACE_OUTER_BOUND ( 'NONE', #8575, .T. ) ;
#3379 = EDGE_CURVE ( 'NONE', #1907, #2249, #6386, .T. ) ;
#3380 = VECTOR ( 'NONE', #5251, 1000.000000000000000 ) ;
#3381 = CARTESIAN_POINT ( 'NONE',  ( 0.000000000000000000, 0.000000000000000000, 120.0000000000000142 ) ) ;
#3382 = EDGE_CURVE ( 'NONE', #3653, #4789, #8210, .T. ) ;
#3383 = VECTOR ( 'NONE', #5122, 1000.000000000000000 ) ;
#3384 = VECTOR ( 'NONE', #2250, 1000.000000000000000 ) ;
#3385 = ORIENTED_EDGE ( 'NONE', *, *, #6459, .F. ) ;
#3386 = LINE ( 'NONE', #5333, #1201 ) ;
#3387 = ORIENTED_EDGE ( 'NONE', *, *, #5809, .T. ) ;
#3388 = LINE ( 'NONE', #7428, #8250 ) ;
#3389 = CARTESIAN_POINT ( 'NONE',  ( 386.6666666666666288, -20.00000000000000000, 162.5000000000000853 ) ) ;
#3390 = DIRECTION ( 'NONE',  ( -0.2508568533328557892, 8.326672684688671588E-17, -0.9680241934662263681 ) ) ;
#3391 = ORIENTED_EDGE ( 'NONE', *, *, #7271, .F. ) ;
#3392 = ORIENTED_EDGE ( 'NONE', *, *, #4510, .F. ) ;
#3393 = MECHANICAL_DESIGN_GEOMETRIC_PRESENTATION_REPRESENTATION (  '', ( #8534 ), #4772 ) ;
#3394 = PLANE ( 'NONE',  #879 ) ;
#3395 = DIRECTION ( 'NONE',  ( 0.000000000000000000, -1.000000000000000000, 0.000000000000000000 ) ) ;
#3396 = VECTOR ( 'NONE', #2589, 1000.000000000000000 ) ;
#3397 = DIRECTION ( 'NONE',  ( 0.000000000000000000, 0.000000000000000000, -1.000000000000000000 ) ) ;
#3398 = ADVANCED_FACE ( 'NONE', ( #6234 ), #845, .T. ) ;
#3399 = CARTESIAN_POINT ( 'NONE',  ( -5.560781378645573980, 0.000000000000000000, -4.000000000000000000 ) ) ;
#3400 = EDGE_LOOP ( 'NONE', ( #4247, #2032 ) ) ;
#3401 = FACE_OUTER_BOUND ( 'NONE', #3304, .T. ) ;
#3402 = ADVANCED_FACE ( 'NONE', ( #977 ), #3588, .F. ) ;
#3403 = ORIENTED_EDGE ( 'NONE', *, *, #1405, .F. ) ;
#3404 = DIRECTION ( 'NONE',  ( 0.000000000000000000, 1.000000000000000000, 0.000000000000000000 ) ) ;
#3405 = VECTOR ( 'NONE', #523, 1000.000000000000000 ) ;
#3406 = CARTESIAN_POINT ( 'NONE',  ( 347.0000000000000000, -4.999999999999998224, 140.0000000000000000 ) ) ;
#3407 = DIRECTION ( 'NONE',  ( -1.734723475976807587E-16, 1.000000000000000000, 0.000000000000000000 ) ) ;
#3408 = VERTEX_POINT ( 'NONE', #3023 ) ;
#3409 = CARTESIAN_POINT ( 'NONE',  ( -20.00000000000000000, 140.0000000000000000, 40.00000000000000000 ) ) ;
#3410 = CARTESIAN_POINT ( 'NONE',  ( -2.100000000000000089, 2.571758278209441957E-16, -4.694516984716113228 ) ) ;
#3411 = CARTESIAN_POINT ( 'NONE',  ( 25.00000000000000000, 2.516649172247811061E-16, -2.055000000000000160 ) ) ;
#3412 = FACE_BOUND ( 'NONE', #4195, .T. ) ;
#3413 = PLANE ( 'NONE',  #1664 ) ;
#3414 = CARTESIAN_POINT ( 'NONE',  ( 8.673617379884035472E-16, 4.618802153517012954, -5.000000000000000000 ) ) ;
#3415 = VERTEX_POINT ( 'NONE', #268 ) ;
#3416 = AXIS2_PLACEMENT_3D ( 'NONE', #3825, #4343, #3046 ) ;
#3417 = ORIENTED_EDGE ( 'NONE', *, *, #5495, .F. ) ;
#3418 = ORIENTED_EDGE ( 'NONE', *, *, #6474, .T. ) ;
#3419 = DIRECTION ( 'NONE',  ( 0.000000000000000000, 0.000000000000000000, -1.000000000000000000 ) ) ;
#3420 = EDGE_CURVE ( 'NONE', #1967, #3415, #2931, .T. ) ;
#3421 = CARTESIAN_POINT ( 'NONE',  ( 5.000000000000000000, 5.000000000000000000, 34.00000000000000711 ) ) ;
#3422 = AXIS2_PLACEMENT_3D ( 'NONE', #5461, #1550, #3425 ) ;
#3423 = CIRCLE ( 'NONE', #503, 2.649999999999985700 ) ;
#3424 = ORIENTED_EDGE ( 'NONE', *, *, #3239, .T. ) ;
#3425 = DIRECTION ( 'NONE',  ( 0.000000000000000000, -0.000000000000000000, 1.000000000000000000 ) ) ;
#3426 = EDGE_CURVE ( 'NONE', #2697, #4430, #5877, .T. ) ;
#3427 = VERTEX_POINT ( 'NONE', #3758 ) ;
#3428 = CARTESIAN_POINT ( 'NONE',  ( 1.747541505913279281, -3.837784562140273081, -3.503702292528912299 ) ) ;
#3429 = DIRECTION ( 'NONE',  ( -1.000000000000000000, -0.000000000000000000, -0.000000000000000000 ) ) ;
#3430 = CONTEXT_DEPENDENT_SHAPE_REPRESENTATION ( #8207, #720 ) ;
#3431 = DIRECTION ( 'NONE',  ( 1.000000000000000000, -1.734723475976806848E-16, 0.000000000000000000 ) ) ;
#3432 = ORIENTED_EDGE ( 'NONE', *, *, #7557, .F. ) ;
#3433 = EDGE_CURVE ( 'NONE', #4319, #101, #1763, .T. ) ;
#3434 = ORIENTED_EDGE ( 'NONE', *, *, #7897, .T. ) ;
#3436 = AXIS2_PLACEMENT_3D ( 'NONE', #2582, #1932, #7101 ) ;
#3435 = DIRECTION ( 'NONE',  ( 0.000000000000000000, 1.000000000000000000, 0.000000000000000000 ) ) ;
#3437 = CARTESIAN_POINT ( 'NONE',  ( 1.567478505476135000E-15, 4.618802153517012954, -3.504269196027527844 ) ) ;
#3438 = CYLINDRICAL_SURFACE ( 'NONE', #1471, 2.649999999999985700 ) ;
#3439 = PRODUCT_DEFINITION_SHAPE ( 'NONE', 'NONE',  #4792 ) ;
#3440 = CARTESIAN_POINT ( 'NONE',  ( 1.360585162435110629, -4.061296242128317857, -3.505054077164905024 ) ) ;
#3441 = VERTEX_POINT ( 'NONE', #4412 ) ;
#3442 = SURFACE_STYLE_FILL_AREA ( #6783 ) ;
#3443 = PLANE ( 'NONE',  #6983 ) ;
#3444 = VERTEX_POINT ( 'NONE', #2584 ) ;
#3445 = ORIENTED_EDGE ( 'NONE', *, *, #2488, .T. ) ;
#3446 = FACE_OUTER_BOUND ( 'NONE', #4309, .T. ) ;
#3447 = CARTESIAN_POINT ( 'NONE',  ( 53.33333333333330017, -15.00000000000000000, 159.8500000000001080 ) ) ;
#3448 = CARTESIAN_POINT ( 'NONE',  ( 5.000000000000000000, -5.000000000000000000, -0.9999999999999940048 ) ) ;
#3449 = ORIENTED_EDGE ( 'NONE', *, *, #6795, .T. ) ;
#3450 = CARTESIAN_POINT ( 'NONE',  ( -4.024497503033519941, 2.323544716729375459, -3.572167766733379768 ) ) ;
#3451 = CARTESIAN_POINT ( 'NONE',  ( 0.000000000000000000, 0.000000000000000000, -14.56854249492377207 ) ) ;
#3452 = ADVANCED_BREP_SHAPE_REPRESENTATION ( '', ( #4654, #594 ), #2832 ) ;
#3453 = EDGE_CURVE ( 'NONE', #3816, #7049, #4303, .T. ) ;
#3454 = EDGE_CURVE ( 'NONE', #5343, #6638, #3474, .T. ) ;
#3455 = EDGE_CURVE ( 'NONE', #5745, #2774, #8504, .T. ) ;
#3456 = CARTESIAN_POINT ( 'NONE',  ( 5.000000000000000000, 134.9989999999999952, 25.00000000000000000 ) ) ;
#3457 = DIRECTION ( 'NONE',  ( 0.000000000000000000, 0.000000000000000000, 1.000000000000000000 ) ) ;
#3458 = FACE_OUTER_BOUND ( 'NONE', #4986, .T. ) ;
#3459 = CARTESIAN_POINT ( 'NONE',  ( 3.999999999999999112, -0.3979232138631231819, -5.929230630780099908E-17 ) ) ;
#3460 = AXIS2_PLACEMENT_3D ( 'NONE', #1346, #5906, #5216 ) ;
#3461 = VERTEX_POINT ( 'NONE', #4369 ) ;
#3462 = EDGE_LOOP ( 'NONE', ( #3774, #4404, #4858, #6975 ) ) ;
#3463 = ORIENTED_EDGE ( 'NONE', *, *, #704, .T. ) ;
#3464 = CARTESIAN_POINT ( 'NONE',  ( 2.500000000000000000, 1.768423874527824902, 1.020999999999999019 ) ) ;
#3465 = FILL_AREA_STYLE ('',( #4244 ) ) ;
#3466 = CIRCLE ( 'NONE', #8197, 2.649999999999985700 ) ;
#3467 = PRODUCT_RELATED_PRODUCT_CATEGORY ( 'part', '', ( #7464 ) ) ;
#3468 = EDGE_LOOP ( 'NONE', ( #3591, #1421, #8093, #8438 ) ) ;
#3469 = DIRECTION ( 'NONE',  ( -0.000000000000000000, -0.000000000000000000, 1.000000000000000000 ) ) ;
#3470 = ORIENTED_EDGE ( 'NONE', *, *, #1548, .F. ) ;
#3471 = CARTESIAN_POINT ( 'NONE',  ( 5.000000000000000000, -5.000000000000000000, -71.99999999999998579 ) ) ;
#3472 =( REPRESENTATION_RELATIONSHIP ('NONE','NONE', #3312, #1533 ) REPRESENTATION_RELATIONSHIP_WITH_TRANSFORMATION ( #2903 )SHAPE_REPRESENTATION_RELATIONSHIP( ) );
#3473 = CARTESIAN_POINT ( 'NONE',  ( -4.999999999999998224, 5.000000000000001776, 140.0000000000000000 ) ) ;
#3474 = CIRCLE ( 'NONE', #1948, 10.00000000000000000 ) ;
#3475 = SHAPE_DEFINITION_REPRESENTATION ( #3439, #872 ) ;
#3476 = CARTESIAN_POINT ( 'NONE',  ( -5.000000000000001776, 5.000000000000001776, -97.99999999999997158 ) ) ;
#3477 = EDGE_LOOP ( 'NONE', ( #6334, #3403, #6903, #556 ) ) ;
#3478 = ORIENTED_EDGE ( 'NONE', *, *, #4246, .F. ) ;
#3479 = LINE ( 'NONE', #149, #2284 ) ;
#3480 = DIRECTION ( 'NONE',  ( -1.000000000000000000, 0.000000000000000000, 0.000000000000000000 ) ) ;
#3481 = VECTOR ( 'NONE', #1630, 1000.000000000000000 ) ;
#3482 = FACE_OUTER_BOUND ( 'NONE', #3230, .T. ) ;
#3483 = CARTESIAN_POINT ( 'NONE',  ( 1.257172072275274388, -3.892973519170983110, -3.433252694550781303 ) ) ;
#3484 = ORIENTED_EDGE ( 'NONE', *, *, #6080, .T. ) ;
#3485 = CARTESIAN_POINT ( 'NONE',  ( 5.000000000000000000, 5.000000000000000000, -71.99999999999998579 ) ) ;
#3486 = CYLINDRICAL_SURFACE ( 'NONE', #1420, 10.00000000000000000 ) ;
#3487 = ORIENTED_EDGE ( 'NONE', *, *, #3672, .T. ) ;
#3488 = VERTEX_POINT ( 'NONE', #7061 ) ;
#3489 = DIRECTION ( 'NONE',  ( -0.000000000000000000, -0.000000000000000000, 1.000000000000000000 ) ) ;
#3490 = CARTESIAN_POINT ( 'NONE',  ( 2.500000000000000000, 2.357898499370433054, -1.951563910473907981E-15 ) ) ;
#3491 = EDGE_CURVE ( 'NONE', #2389, #848, #1105, .T. ) ;
#3492 = EDGE_CURVE ( 'NONE', #7186, #4726, #6406, .T. ) ;
#3493 = FACE_OUTER_BOUND ( 'NONE', #2183, .T. ) ;
#3494 = CARTESIAN_POINT ( 'NONE',  ( 5.000000000000000000, 5.000000000000000000, 148.0000000000000284 ) ) ;
#3495 = ORIENTED_EDGE ( 'NONE', *, *, #5359, .F. ) ;
#3496 = FACE_BOUND ( 'NONE', #6985, .T. ) ;
#3497 = CARTESIAN_POINT ( 'NONE',  ( 24.55500000000002103, 0.000000000000000000, 2.500000000000001332 ) ) ;
#3498 = DIRECTION ( 'NONE',  ( 1.000000000000000000, 0.000000000000000000, 0.000000000000000000 ) ) ;
#3499 = DIRECTION ( 'NONE',  ( -0.000000000000000000, -0.000000000000000000, 1.000000000000000000 ) ) ;
#3500 = DIRECTION ( 'NONE',  ( 0.000000000000000000, 0.000000000000000000, 1.000000000000000000 ) ) ;
#3501 = PLANE ( 'NONE',  #8025 ) ;
#3502 = ADVANCED_FACE ( 'NONE', ( #5753 ), #5104, .T. ) ;
#3503 = EDGE_LOOP ( 'NONE', ( #7128, #6767, #6332, #7667 ) ) ;
#3504 = ORIENTED_EDGE ( 'NONE', *, *, #7, .F. ) ;
#3505 = VERTEX_POINT ( 'NONE', #5227 ) ;
#3506 = LINE ( 'NONE', #97, #7277 ) ;
#3507 = PRODUCT_DEFINITION_SHAPE ( 'NONE', 'NONE',  #8607 ) ;
#3508 = VERTEX_POINT ( 'NONE', #3110 ) ;
#3509 = PLANE ( 'NONE',  #4812 ) ;
#3510 = VECTOR ( 'NONE', #2718, 1000.000000000000000 ) ;
#3511 = VERTEX_POINT ( 'NONE', #2508 ) ;
#3512 = FACE_OUTER_BOUND ( 'NONE', #4512, .T. ) ;
#3513 = FACE_OUTER_BOUND ( 'NONE', #7873, .T. ) ;
#3514 = ITEM_DEFINED_TRANSFORMATION ( 'NONE', 'NONE', #1845,  #594 ) ;
#3515 = PRODUCT_DEFINITION ( 'UNKNOWN', '', #440, #4548 ) ;
#3516 = ORIENTED_EDGE ( 'NONE', *, *, #4245, .F. ) ;
#3517 = VECTOR ( 'NONE', #1880, 1000.000000000000000 ) ;
#3518 = EDGE_LOOP ( 'NONE', ( #3147, #2033, #6113, #4203 ) ) ;
#3519 = DIRECTION ( 'NONE',  ( 0.000000000000000000, 0.000000000000000000, -1.000000000000000000 ) ) ;
#3520 = CARTESIAN_POINT ( 'NONE',  ( -30.00000000000002842, -20.00000000000000000, 140.0000000000000000 ) ) ;
#3521 = CIRCLE ( 'NONE', #3241, 10.00000000000000000 ) ;
#3522 = AXIS2_PLACEMENT_3D ( 'NONE', #5077, #3129, #3775 ) ;
#3523 = AXIS2_PLACEMENT_3D ( 'NONE', #6517, #2694, #7872 ) ;
#3524 = CARTESIAN_POINT ( 'NONE',  ( 1.411581201560190495E-15, 4.862606272033091592, -3.745885042887436622 ) ) ;
#3525 = CARTESIAN_POINT ( 'NONE',  ( 0.6920835326022565237, 4.454600218803884459, -3.597382984111579862 ) ) ;
#3526 = ORIENTED_EDGE ( 'NONE', *, *, #7820, .F. ) ;
#3527 = FILL_AREA_STYLE_COLOUR ( '', #4599 ) ;
#3528 = DIRECTION ( 'NONE',  ( 0.000000000000000000, 0.000000000000000000, 1.000000000000000000 ) ) ;
#3529 = VERTEX_POINT ( 'NONE', #4530 ) ;
#3530 = CARTESIAN_POINT ( 'NONE',  ( 2.100000000000000089, 0.000000000000000000, -5.000000000000000000 ) ) ;
#3531 = LINE ( 'NONE', #6178, #898 ) ;
#3532 = AXIS2_PLACEMENT_3D ( 'NONE', #6197, #2245, #1371 ) ;
#3533 = DIRECTION ( 'NONE',  ( 0.000000000000000000, 0.000000000000000000, 1.000000000000000000 ) ) ;
#3534 = EDGE_CURVE ( 'NONE', #2469, #3441, #6364, .T. ) ;
#3535 = LINE ( 'NONE', #2969, #2071 ) ;
#3536 = EDGE_LOOP ( 'NONE', ( #1551, #7264, #6541, #7043 ) ) ;
#3537 = DIRECTION ( 'NONE',  ( 0.000000000000000000, 0.000000000000000000, 1.000000000000000000 ) ) ;
#3538 = EDGE_CURVE ( 'NONE', #1033, #1781, #1893, .T. ) ;
#3539 = VECTOR ( 'NONE', #3616, 1000.000000000000000 ) ;
#3540 = LINE ( 'NONE', #928, #3934 ) ;
#3541 = ADVANCED_FACE ( 'NONE', ( #404 ), #7769, .F. ) ;
#3542 = DIRECTION ( 'NONE',  ( -1.000000000000000000, 0.000000000000000000, 0.000000000000000000 ) ) ;
#3543 = CARTESIAN_POINT ( 'NONE',  ( -5.000000000000000000, -5.000000000000000000, 34.00000000000000711 ) ) ;
#3544 = CARTESIAN_POINT ( 'NONE',  ( -5.000000000000001776, 5.000000000000001776, 140.0000000000000000 ) ) ;
#3545 = CARTESIAN_POINT ( 'NONE',  ( -30.00000000000000000, 15.00000000000000000, 140.0000000000000000 ) ) ;
#3546 = ORIENTED_EDGE ( 'NONE', *, *, #3856, .F. ) ;
#3547 = ORIENTED_EDGE ( 'NONE', *, *, #4213, .F. ) ;
#3548 = ORIENTED_EDGE ( 'NONE', *, *, #7672, .F. ) ;
#3549 = CYLINDRICAL_SURFACE ( 'NONE', #3532, 2.649999999999985700 ) ;
#3550 = DIRECTION ( 'NONE',  ( 0.000000000000000000, -1.000000000000000000, 0.000000000000000000 ) ) ;
#3551 = ORIENTED_EDGE ( 'NONE', *, *, #1889, .F. ) ;
#3552 = AXIS2_PLACEMENT_3D ( 'NONE', #1210, #7082, #7166 ) ;
#3553 = LINE ( 'NONE', #2304, #7311 ) ;
#3554 = ORIENTED_EDGE ( 'NONE', *, *, #5769, .T. ) ;
#3555 = DIRECTION ( 'NONE',  ( -1.000000000000000000, 0.000000000000000000, 0.000000000000000000 ) ) ;
#3556 = CARTESIAN_POINT ( 'NONE',  ( 470.0000000000000000, -15.00000000000000000, 180.0000000000000284 ) ) ;
#3557 = ORIENTED_EDGE ( 'NONE', *, *, #3938, .F. ) ;
#3558 = ORIENTED_EDGE ( 'NONE', *, *, #880, .F. ) ;
#3559 = CARTESIAN_POINT ( 'NONE',  ( 0.000000000000000000, -1.178949249685218303, -2.041999999999998039 ) ) ;
#3560 = DIRECTION ( 'NONE',  ( -0.000000000000000000, -0.000000000000000000, -1.000000000000000000 ) ) ;
#3561 = AXIS2_PLACEMENT_3D ( 'NONE', #4899, #8220, #812 ) ;
#3562 = ADVANCED_FACE ( 'NONE', ( #3889 ), #3716, .T. ) ;
#3563 = AXIS2_PLACEMENT_3D ( 'NONE', #2165, #7429, #194 ) ;
#3564 = ADVANCED_FACE ( 'NONE', ( #3069 ), #5710, .F. ) ;
#3565 = EDGE_CURVE ( 'NONE', #6024, #3923, #5268, .T. ) ;
#3566 = LINE ( 'NONE', #1655, #2054 ) ;
#3567 = CARTESIAN_POINT ( 'NONE',  ( 4.141042297810615835, -2.227970268150433863, -3.687027686973623819 ) ) ;
#3568 = ORIENTED_EDGE ( 'NONE', *, *, #4284, .T. ) ;
#3569 = PRESENTATION_LAYER_ASSIGNMENT (  '', '', ( #3155 ) ) ;
#3570 =( NAMED_UNIT ( * ) SI_UNIT ( $, .STERADIAN. ) SOLID_ANGLE_UNIT ( ) );
#3571 = CARTESIAN_POINT ( 'NONE',  ( 470.0000000000000000, 15.00000000000000000, 145.0000000000000284 ) ) ;
#3572 = ORIENTED_EDGE ( 'NONE', *, *, #8476, .F. ) ;
#3573 = DIRECTION ( 'NONE',  ( 1.000000000000000000, 0.000000000000000000, 0.000000000000000000 ) ) ;
#3574 = LINE ( 'NONE', #6223, #6311 ) ;
#3575 = AXIS2_PLACEMENT_3D ( 'NONE', #1764, #978, #6454 ) ;
#3576 = VECTOR ( 'NONE', #2479, 1000.000000000000000 ) ;
#3577 = EDGE_CURVE ( 'NONE', #6119, #7579, #7650, .T. ) ;
#3578 = CARTESIAN_POINT ( 'NONE',  ( -2.688821387764050996E-14, -4.618802153517012954, -0.4999999999999995559 ) ) ;
#3579 = CARTESIAN_POINT ( 'NONE',  ( -5.000000000000000000, -5.000000000000000000, 148.0000000000000284 ) ) ;
#3580 = VERTEX_POINT ( 'NONE', #5310 ) ;
#3581 = CYLINDRICAL_SURFACE ( 'NONE', #4441, 2.649999999999985700 ) ;
#3582 = CARTESIAN_POINT ( 'NONE',  ( 88.00000000000000000, -20.00000000000000000, -119.1814250403154745 ) ) ;
#3583 = DIRECTION ( 'NONE',  ( -0.000000000000000000, 1.000000000000000000, -0.000000000000000000 ) ) ;
#3584 = VECTOR ( 'NONE', #7439, 1000.000000000000000 ) ;
#3585 =( REPRESENTATION_RELATIONSHIP ('NONE','NONE', #3312, #1479 ) REPRESENTATION_RELATIONSHIP_WITH_TRANSFORMATION ( #677 )SHAPE_REPRESENTATION_RELATIONSHIP( ) );
#3586 = DIRECTION ( 'NONE',  ( 0.000000000000000000, 1.000000000000000000, 0.000000000000000000 ) ) ;
#3587 = EDGE_CURVE ( 'NONE', #3640, #8324, #4659, .T. ) ;
#3588 = PLANE ( 'NONE',  #411 ) ;
#3589 = LINE ( 'NONE', #3545, #4667 ) ;
#3590 = ORIENTED_EDGE ( 'NONE', *, *, #3119, .T. ) ;
#3591 = ORIENTED_EDGE ( 'NONE', *, *, #3594, .T. ) ;
#3592 = VERTEX_POINT ( 'NONE', #6004 ) ;
#3593 = LINE ( 'NONE', #983, #2566 ) ;
#3594 = EDGE_CURVE ( 'NONE', #4134, #2451, #125, .T. ) ;
#3595 = AXIS2_PLACEMENT_3D ( 'NONE', #8496, #2537, #6313 ) ;
#3596 = EDGE_CURVE ( 'NONE', #926, #3371, #4874, .T. ) ;
#3597 = ORIENTED_EDGE ( 'NONE', *, *, #7668, .F. ) ;
#3598 = CARTESIAN_POINT ( 'NONE',  ( -5.000000000000001776, 5.000000000000001776, 148.0000000000000284 ) ) ;
#3599 = ORIENTED_EDGE ( 'NONE', *, *, #7, .T. ) ;
#3600 = LINE ( 'NONE', #7515, #6199 ) ;
#3601 = LINE ( 'NONE', #7812, #5445 ) ;
#3602 = VERTEX_POINT ( 'NONE', #1313 ) ;
#3603 = ORIENTED_EDGE ( 'NONE', *, *, #4936, .T. ) ;
#3604 = CARTESIAN_POINT ( 'NONE',  ( -20.00000000000000000, 2.449293598294706513E-15, -154.5685424949238040 ) ) ;
#3605 = VECTOR ( 'NONE', #2027, 1000.000000000000000 ) ;
#3606 = CARTESIAN_POINT ( 'NONE',  ( 347.0000000000000000, 5.000000000000001776, 140.0000000000000000 ) ) ;
#3607 = CARTESIAN_POINT ( 'NONE',  ( -3.510273485745307287, -2.827716139362669967, -3.610536846335890004 ) ) ;
#3608 = VECTOR ( 'NONE', #8470, 1000.000000000000000 ) ;
#3609 = VERTEX_POINT ( 'NONE', #2757 ) ;
#3610 = ADVANCED_FACE ( 'NONE', ( #7406 ), #5356, .F. ) ;
#3611 = SURFACE_STYLE_USAGE ( .BOTH. , #2222 ) ;
#3612 = CARTESIAN_POINT ( 'NONE',  ( 0.000000000000000000, 0.000000000000000000, -0.2800830152838844622 ) ) ;
#3613 = VERTEX_POINT ( 'NONE', #4617 ) ;
#3614 = ORIENTED_EDGE ( 'NONE', *, *, #6832, .F. ) ;
#3615 = LINE ( 'NONE', #6124, #1156 ) ;
#3616 = DIRECTION ( 'NONE',  ( 1.000000000000000000, 0.000000000000000000, 0.000000000000000000 ) ) ;
#3617 = CARTESIAN_POINT ( 'NONE',  ( 5.000000000000000000, 5.000000000000000000, -36.00000000000000000 ) ) ;
#3618 = FACE_BOUND ( 'NONE', #8040, .T. ) ;
#3619 = EDGE_LOOP ( 'NONE', ( #7531, #8300, #5892, #1211, #1027 ) ) ;
#3620 = CARTESIAN_POINT ( 'NONE',  ( 53.33333333333330017, -15.00000000000000000, 162.5000000000000853 ) ) ;
#3621 = CARTESIAN_POINT ( 'NONE',  ( -10.00000000000000000, 1.224646799147353059E-15, -27.99999999999999645 ) ) ;
#3622 = CYLINDRICAL_SURFACE ( 'NONE', #7968, 2.649999999999985700 ) ;
#3623 = LINE ( 'NONE', #8251, #4579 ) ;
#3624 = DIRECTION ( 'NONE',  ( -1.000000000000000000, 1.734723475976806848E-16, -0.000000000000000000 ) ) ;
#3625 = SURFACE_STYLE_USAGE ( .BOTH. , #2932 ) ;
#3626 = ORIENTED_EDGE ( 'NONE', *, *, #5135, .T. ) ;
#3627 = ORIENTED_EDGE ( 'NONE', *, *, #7979, .T. ) ;
#3628 = ORIENTED_EDGE ( 'NONE', *, *, #1952, .F. ) ;
#3629 = DIRECTION ( 'NONE',  ( -0.000000000000000000, -0.000000000000000000, 1.000000000000000000 ) ) ;
#3630 = CARTESIAN_POINT ( 'NONE',  ( 352.0000000000000000, -25.00000000000000000, -16.23142504031546807 ) ) ;
#3631 =( REPRESENTATION_RELATIONSHIP ('NONE','NONE', #3312, #4706 ) REPRESENTATION_RELATIONSHIP_WITH_TRANSFORMATION ( #3819 )SHAPE_REPRESENTATION_RELATIONSHIP( ) );
#3632 = STYLED_ITEM ( 'NONE', ( #2317 ), #3979 ) ;
#3633 = ORIENTED_EDGE ( 'NONE', *, *, #2070, .T. ) ;
#3634 = DIRECTION ( 'NONE',  ( 0.000000000000000000, 0.000000000000000000, 1.000000000000000000 ) ) ;
#3635 = EDGE_CURVE ( 'NONE', #6857, #7956, #8482, .T. ) ;
#3636 = EDGE_LOOP ( 'NONE', ( #3568, #1385 ) ) ;
#3637 = FILL_AREA_STYLE ('',( #1688 ) ) ;
#3638 = DIRECTION ( 'NONE',  ( 0.000000000000000000, 0.000000000000000000, -1.000000000000000000 ) ) ;
#3639 = EDGE_CURVE ( 'NONE', #5674, #1367, #5266, .T. ) ;
#3640 = VERTEX_POINT ( 'NONE', #1267 ) ;
#3641 = EDGE_LOOP ( 'NONE', ( #5824, #5975, #1131, #7539 ) ) ;
#3642 = CYLINDRICAL_SURFACE ( 'NONE', #2288, 10.00000000000000000 ) ;
#3643 = CARTESIAN_POINT ( 'NONE',  ( 0.000000000000000000, 0.000000000000000000, 0.000000000000000000 ) ) ;
#3644 =( GEOMETRIC_REPRESENTATION_CONTEXT ( 3 ) GLOBAL_UNCERTAINTY_ASSIGNED_CONTEXT ( ( #6061 ) ) GLOBAL_UNIT_ASSIGNED_CONTEXT ( ( #4534, #5593, #7612 ) ) REPRESENTATION_CONTEXT ( 'NONE', 'WORKASPACE' ) );
#3645 = EDGE_CURVE ( 'NONE', #1565, #6851, #573, .T. ) ;
#3646 = CARTESIAN_POINT ( 'NONE',  ( -10.00000000000000000, 1.224646799147353256E-15, -63.99999999999997158 ) ) ;
#3647 = VECTOR ( 'NONE', #8122, 1000.000000000000000 ) ;
#3648 = DIRECTION ( 'NONE',  ( 0.000000000000000000, -1.000000000000000000, 0.000000000000000000 ) ) ;
#3649 = CYLINDRICAL_SURFACE ( 'NONE', #406, 2.649999999999985700 ) ;
#3650 = EDGE_LOOP ( 'NONE', ( #4542, #4088 ) ) ;
#3651 = CARTESIAN_POINT ( 'NONE',  ( 88.00000000000000000, 0.000000000000000000, 0.000000000000000000 ) ) ;
#3652 = DIRECTION ( 'NONE',  ( -1.734723475976807341E-16, 1.000000000000000000, 0.000000000000000000 ) ) ;
#3653 = VERTEX_POINT ( 'NONE', #755 ) ;
#3654 = ORIENTED_EDGE ( 'NONE', *, *, #2097, .T. ) ;
#3655 = VECTOR ( 'NONE', #2607, 1000.000000000000000 ) ;
#3656 = CARTESIAN_POINT ( 'NONE',  ( -5.000000000000001776, 5.000000000000001776, -97.99999999999997158 ) ) ;
#3657 = CARTESIAN_POINT ( 'NONE',  ( 5.000000000000000000, -5.000000000000000000, -36.00000000000000000 ) ) ;
#3658 = AXIS2_PLACEMENT_3D ( 'NONE', #2124, #6073, #7521 ) ;
#3659 = VECTOR ( 'NONE', #4399, 1000.000000000000000 ) ;
#3660 = ADVANCED_FACE ( 'NONE', ( #2716 ), #2065, .F. ) ;
#3661 = VECTOR ( 'NONE', #3550, 1000.000000000000000 ) ;
#3662 = COLOUR_RGB ( '',0.8941176470588234615, 0.8941176470588234615, 0.8941176470588234615 ) ;
#3663 = CARTESIAN_POINT ( 'NONE',  ( 386.6666666666666288, -14.99999999999999822, 162.5000000000000853 ) ) ;
#3664 = DIRECTION ( 'NONE',  ( -1.000000000000000000, -0.000000000000000000, -0.000000000000000000 ) ) ;
#3665 = ORIENTED_EDGE ( 'NONE', *, *, #1573, .T. ) ;
#3666 = FACE_BOUND ( 'NONE', #4928, .T. ) ;
#3667 = SURFACE_SIDE_STYLE ('',( #2972 ) ) ;
#3668 = ORIENTED_EDGE ( 'NONE', *, *, #939, .T. ) ;
#3669 = CARTESIAN_POINT ( 'NONE',  ( 1.274258131564866448, 3.883108878240963513, -3.220599429844046568 ) ) ;
#3670 = CIRCLE ( 'NONE', #1442, 2.649999999999985700 ) ;
#3671 = CARTESIAN_POINT ( 'NONE',  ( 5.000000000000000000, -5.000000000000000000, 140.0000000000000000 ) ) ;
#3672 = EDGE_CURVE ( 'NONE', #5766, #1691, #4575, .T. ) ;
#3673 = ADVANCED_FACE ( 'NONE', ( #4710 ), #2019, .F. ) ;
#3674 = CYLINDRICAL_SURFACE ( 'NONE', #974, 10.00000000000000000 ) ;
#3675 = EDGE_CURVE ( 'NONE', #3060, #8171, #1356, .T. ) ;
#3676 = CARTESIAN_POINT ( 'NONE',  ( -3.453038570459499024, -2.625189405340453419, -3.535263753545272891 ) ) ;
#3677 = CARTESIAN_POINT ( 'NONE',  ( -4.000000000000000000, -0.8382240730041925492, -3.220610619767135141 ) ) ;
#3678 = VECTOR ( 'NONE', #5048, 1000.000000000000000 ) ;
#3679 = ORIENTED_EDGE ( 'NONE', *, *, #8572, .F. ) ;
#3680 = VERTEX_POINT ( 'NONE', #1447 ) ;
#3681 = CARTESIAN_POINT ( 'NONE',  ( 3.355112389629172576, -2.681727112203168950, -0.2256878752776777242 ) ) ;
#3682 = CARTESIAN_POINT ( 'NONE',  ( -1.240299975428113101E-15, -4.647091401871173311, -3.572172305156514849 ) ) ;
#3683 = CARTESIAN_POINT ( 'NONE',  ( 0.000000000000000000, 0.000000000000000000, 7.000000000000006217 ) ) ;
#3684 = ORIENTED_EDGE ( 'NONE', *, *, #7315, .F. ) ;
#3685 = DIRECTION ( 'NONE',  ( 1.000000000000000000, 0.000000000000000000, 0.000000000000000000 ) ) ;
#3686 = EDGE_LOOP ( 'NONE', ( #8514, #4305, #7468, #875 ) ) ;
#3687 = DIRECTION ( 'NONE',  ( -1.000000000000000000, 1.734723475976806848E-16, -0.000000000000000000 ) ) ;
#3688 = ORIENTED_EDGE ( 'NONE', *, *, #880, .T. ) ;
#3689 = EDGE_CURVE ( 'NONE', #147, #3488, #7363, .T. ) ;
#3690 = VERTEX_POINT ( 'NONE', #799 ) ;
#3691 = DIRECTION ( 'NONE',  ( -0.000000000000000000, 0.000000000000000000, 1.000000000000000000 ) ) ;
#3692 = CARTESIAN_POINT ( 'NONE',  ( 0.000000000000000000, 0.000000000000000000, -97.99999999999997158 ) ) ;
#3693 = LINE ( 'NONE', #6432, #5772 ) ;
#3694 = DIRECTION ( 'NONE',  ( -0.000000000000000000, 1.000000000000000000, -0.000000000000000000 ) ) ;
#3695 = ORIENTED_EDGE ( 'NONE', *, *, #2131, .T. ) ;
#3696 = ADVANCED_FACE ( 'NONE', ( #1400, #6702 ), #2796, .T. ) ;
#3697 = DIRECTION ( 'NONE',  ( 0.000000000000000000, 0.000000000000000000, 1.000000000000000000 ) ) ;
#3698 = DIRECTION ( 'NONE',  ( -1.000000000000000000, 0.000000000000000000, 0.000000000000000000 ) ) ;
#3699 = VERTEX_POINT ( 'NONE', #4573 ) ;
#3700 = VERTEX_POINT ( 'NONE', #7227 ) ;
#3701 = VECTOR ( 'NONE', #6398, 1000.000000000000000 ) ;
#3702 = CARTESIAN_POINT ( 'NONE',  ( 93.00000000000000000, -4.999999999999998224, 145.0000000000000284 ) ) ;
#3703 = DIRECTION ( 'NONE',  ( -1.000000000000000000, 0.000000000000000000, 0.000000000000000000 ) ) ;
#3704 = VECTOR ( 'NONE', #1686, 1000.000000000000000 ) ;
#3705 = DIRECTION ( 'NONE',  ( -1.000000000000000000, 0.000000000000000000, -0.000000000000000000 ) ) ;
#3706 = AXIS2_PLACEMENT_3D ( 'NONE', #4121, #103, #815 ) ;
#3707 = DIRECTION ( 'NONE',  ( -0.000000000000000000, 1.000000000000000000, -0.000000000000000000 ) ) ;
#3708 = VERTEX_POINT ( 'NONE', #3277 ) ;
#3709 = CARTESIAN_POINT ( 'NONE',  ( 170.9999999999999716, -4.999999999999998224, 139.9990000000000236 ) ) ;
#3710 = VERTEX_POINT ( 'NONE', #5916 ) ;
#3711 = CARTESIAN_POINT ( 'NONE',  ( 0.5636800770130377947, 4.293361309317166530, -3.531542292954102713 ) ) ;
#3712 = COLOUR_RGB ( '',0.8941176470588234615, 0.8941176470588234615, 0.8941176470588234615 ) ;
#3713 = VECTOR ( 'NONE', #7188, 1000.000000000000000 ) ;
#3714 = DIRECTION ( 'NONE',  ( -0.000000000000000000, -0.000000000000000000, 1.000000000000000000 ) ) ;
#3715 = LINE ( 'NONE', #5059, #1821 ) ;
#3716 = CYLINDRICAL_SURFACE ( 'NONE', #5134, 20.00000000000000000 ) ;
#3717 = DIRECTION ( 'NONE',  ( 1.000000000000000000, -1.734723475976806848E-16, 0.000000000000000000 ) ) ;
#3718 = ORIENTED_EDGE ( 'NONE', *, *, #1149, .T. ) ;
#3719 = EDGE_CURVE ( 'NONE', #7552, #1114, #5819, .T. ) ;
#3720 = ADVANCED_FACE ( 'NONE', ( #6134, #2971, #6839, #2191, #3666, #6227, #8119 ), #970, .T. ) ;
#3721 = ORIENTED_EDGE ( 'NONE', *, *, #2809, .F. ) ;
#3722 = DIRECTION ( 'NONE',  ( 1.734723475976807587E-16, 0.000000000000000000, -1.000000000000000000 ) ) ;
#3723 = DIRECTION ( 'NONE',  ( 0.000000000000000000, 0.000000000000000000, 1.000000000000000000 ) ) ;
#3724 = EDGE_LOOP ( 'NONE', ( #7143, #8545, #7925, #6967 ) ) ;
#3725 = DIRECTION ( 'NONE',  ( 0.000000000000000000, 0.000000000000000000, 1.000000000000000000 ) ) ;
#3726 = EDGE_LOOP ( 'NONE', ( #6175, #2523 ) ) ;
#3727 = SURFACE_STYLE_FILL_AREA ( #3637 ) ;
#3728 = PLANE ( 'NONE',  #7317 ) ;
#3729 = ORIENTED_EDGE ( 'NONE', *, *, #5962, .T. ) ;
#3730 = ORIENTED_EDGE ( 'NONE', *, *, #7179, .F. ) ;
#3731 = DIRECTION ( 'NONE',  ( -0.000000000000000000, -0.000000000000000000, -1.000000000000000000 ) ) ;
#3732 = EDGE_CURVE ( 'NONE', #6221, #7614, #1382, .T. ) ;
#3733 = DIRECTION ( 'NONE',  ( 1.000000000000000000, 0.000000000000000000, 0.000000000000000000 ) ) ;
#3734 = VECTOR ( 'NONE', #4650, 1000.000000000000227 ) ;
#3735 = CARTESIAN_POINT ( 'NONE',  ( 20.00000000000000000, 175.0000000000000284, 5.000000000000000000 ) ) ;
#3736 = EDGE_LOOP ( 'NONE', ( #6828, #2001, #3875, #5931 ) ) ;
#3737 = AXIS2_PLACEMENT_3D ( 'NONE', #2762, #5407, #8081 ) ;
#3738 = CARTESIAN_POINT ( 'NONE',  ( 176.0000000000000000, -20.00000000000000000, 70.86857495968455112 ) ) ;
#3739 = DIRECTION ( 'NONE',  ( 1.000000000000000000, 0.000000000000000000, 0.000000000000000000 ) ) ;
#3740 = VERTEX_POINT ( 'NONE', #8158 ) ;
#3741 = ORIENTED_EDGE ( 'NONE', *, *, #1895, .F. ) ;
#3742 = CARTESIAN_POINT ( 'NONE',  ( 5.000000000000000000, 5.000000000000000000, 140.0000000000000000 ) ) ;
#3743 = DIRECTION ( 'NONE',  ( 1.000000000000000000, 1.734723475976807587E-16, 0.000000000000000000 ) ) ;
#3744 = VECTOR ( 'NONE', #7021, 1000.000000000000000 ) ;
#3745 = CARTESIAN_POINT ( 'NONE',  ( -10.00000000000000000, 1.224646799147353256E-15, 140.0000000000000000 ) ) ;
#3746 = DIRECTION ( 'NONE',  ( -0.5000000000000016653, 0.8660254037844378194, 0.000000000000000000 ) ) ;
#3747 = ORIENTED_EDGE ( 'NONE', *, *, #3832, .F. ) ;
#3748 = EDGE_CURVE ( 'NONE', #8592, #5790, #6965, .T. ) ;
#3749 = ORIENTED_EDGE ( 'NONE', *, *, #823, .T. ) ;
#3750 =( REPRESENTATION_RELATIONSHIP ('NONE','NONE', #3312, #2984 ) REPRESENTATION_RELATIONSHIP_WITH_TRANSFORMATION ( #1646 )SHAPE_REPRESENTATION_RELATIONSHIP( ) );
#3751 = AXIS2_PLACEMENT_3D ( 'NONE', #2591, #5234, #2674 ) ;
#3752 = FACE_OUTER_BOUND ( 'NONE', #8259, .T. ) ;
#3753 = ADVANCED_FACE ( 'NONE', ( #261 ), #348, .F. ) ;
#3754 = ADVANCED_FACE ( 'NONE', ( #4969 ), #3581, .F. ) ;
#3755 = FACE_BOUND ( 'NONE', #4605, .T. ) ;
#3756 = AXIS2_PLACEMENT_3D ( 'NONE', #5776, #6305, #1746 ) ;
#3757 = CARTESIAN_POINT ( 'NONE',  ( 2.500000000000000000, -1.178949249685218303, -2.041999999999998039 ) ) ;
#3758 = CARTESIAN_POINT ( 'NONE',  ( -5.000000000000001776, 5.000000000000001776, 148.0000000000000284 ) ) ;
#3759 = CARTESIAN_POINT ( 'NONE',  ( -4.211405944401398038, -2.460460786169389902, -3.751298493805494072 ) ) ;
#3760 = ORIENTED_EDGE ( 'NONE', *, *, #1575, .F. ) ;
#3761 = SURFACE_STYLE_FILL_AREA ( #1109 ) ;
#3762 = DIRECTION ( 'NONE',  ( -1.000000000000000000, 0.000000000000000000, 0.000000000000000000 ) ) ;
#3763 = CARTESIAN_POINT ( 'NONE',  ( 2.500000000000000000, 1.178949249685218525, 2.041999999999999371 ) ) ;
#3764 = DIRECTION ( 'NONE',  ( -1.734723475976807587E-16, 1.000000000000000000, 0.000000000000000000 ) ) ;
#3765 = UNCERTAINTY_MEASURE_WITH_UNIT (LENGTH_MEASURE( 1.000000000000000082E-05 ), #3146, 'distance_accuracy_value', 'NONE');
#3766 = ADVANCED_FACE ( 'NONE', ( #6270, #5571, #5442, #3496, #7538, #2925 ), #4274, .F. ) ;
#3767 = ORIENTED_EDGE ( 'NONE', *, *, #7899, .F. ) ;
#3768 = DIRECTION ( 'NONE',  ( -0.000000000000000000, 1.000000000000000000, -0.000000000000000000 ) ) ;
#3769 = EDGE_LOOP ( 'NONE', ( #7771, #6587, #4466, #6991 ) ) ;
#3770 = ADVANCED_FACE ( 'NONE', ( #7449 ), #7630, .T. ) ;
#3771 = PLANE ( 'NONE',  #6486 ) ;
#3772 = ITEM_DEFINED_TRANSFORMATION ( 'NONE', 'NONE', #5853,  #594 ) ;
#3773 = ORIENTED_EDGE ( 'NONE', *, *, #706, .F. ) ;
#3774 = ORIENTED_EDGE ( 'NONE', *, *, #2663, .T. ) ;
#3775 = DIRECTION ( 'NONE',  ( -1.000000000000000000, 1.734723475976807587E-16, 0.000000000000000000 ) ) ;
#3776 = CARTESIAN_POINT ( 'NONE',  ( -5.000000000000001776, 5.000000000000001776, 140.0000000000000000 ) ) ;
#3777 = STYLED_ITEM ( 'NONE', ( #5219 ), #1900 ) ;
#3778 = B_SPLINE_CURVE_WITH_KNOTS ( 'NONE', 3,
 ( #5689, #2399, #1742, #1787, #4389 ),
 .UNSPECIFIED., .F., .F.,
 ( 4, 1, 4 ),
 ( 0.000000000000000000, 0.002309401076758505790, 0.004618802153517011580 ),
 .UNSPECIFIED. ) ;
#3779 = CARTESIAN_POINT ( 'NONE',  ( 5.000000000000000000, -5.000000000000000000, -135.0000000000000000 ) ) ;
#3780 = PRODUCT_DEFINITION ( 'UNKNOWN', '', #2948, #3954 ) ;
#3781 = ORIENTED_EDGE ( 'NONE', *, *, #976, .T. ) ;
#3782 = ADVANCED_FACE ( 'NONE', ( #3512 ), #1552, .T. ) ;
#3783 = DIRECTION ( 'NONE',  ( 6.123233995736766036E-17, -1.000000000000000000, 0.000000000000000000 ) ) ;
#3784 = CARTESIAN_POINT ( 'NONE',  ( 0.000000000000000000, 157.5000000000000284, 5.000000000000000000 ) ) ;
#3785 = ORIENTED_EDGE ( 'NONE', *, *, #363, .T. ) ;
#3786 = CIRCLE ( 'NONE', #3233, 4.250000000000000000 ) ;
#3787 = ORIENTED_EDGE ( 'NONE', *, *, #5195, .F. ) ;
#3788 = CARTESIAN_POINT ( 'NONE',  ( 219.9999999999999716, -15.00000000000000000, 165.1500000000000625 ) ) ;
#3789 = CARTESIAN_POINT ( 'NONE',  ( 5.384454397937118664, 0.000000000000000000, -5.000000000000000000 ) ) ;
#3790 = ORIENTED_EDGE ( 'NONE', *, *, #4842, .F. ) ;
#3791 = DIRECTION ( 'NONE',  ( 0.000000000000000000, 0.000000000000000000, 1.000000000000000000 ) ) ;
#3792 = CYLINDRICAL_SURFACE ( 'NONE', #250, 4.250000000000000000 ) ;
#3793 = ORIENTED_EDGE ( 'NONE', *, *, #2375, .T. ) ;
#3794 = AXIS2_PLACEMENT_3D ( 'NONE', #801, #7499, #3542 ) ;
#3795 =( NAMED_UNIT ( * ) SI_UNIT ( $, .STERADIAN. ) SOLID_ANGLE_UNIT ( ) );
#3796 = EDGE_LOOP ( 'NONE', ( #1603, #2651, #4939, #2294 ) ) ;
#3797 = FACE_OUTER_BOUND ( 'NONE', #2346, .T. ) ;
#3798 = EDGE_CURVE ( 'NONE', #2255, #5002, #5489, .T. ) ;
#3799 = AXIS2_PLACEMENT_3D ( 'NONE', #5696, #5780, #1749 ) ;
#3800 = VECTOR ( 'NONE', #6337, 1000.000000000000000 ) ;
#3801 = VECTOR ( 'NONE', #1212, 1000.000000000000000 ) ;
#3802 = EDGE_CURVE ( 'NONE', #926, #1258, #1766, .T. ) ;
#3803 = CARTESIAN_POINT ( 'NONE',  ( 434.9999999999999432, 5.000000000000001776, 145.0000000000000284 ) ) ;
#3804 = CARTESIAN_POINT ( 'NONE',  ( 0.000000000000000000, 0.000000000000000000, 120.0000000000000142 ) ) ;
#3805 = EDGE_CURVE ( 'NONE', #5804, #3177, #1581, .T. ) ;
#3806 = DIRECTION ( 'NONE',  ( -0.000000000000000000, -0.000000000000000000, 1.000000000000000000 ) ) ;
#3807 = VERTEX_POINT ( 'NONE', #8244 ) ;
#3808 = EDGE_CURVE ( 'NONE', #1549, #7220, #2283, .T. ) ;
#3809 = VECTOR ( 'NONE', #1155, 1000.000000000000000 ) ;
#3810 =( GEOMETRIC_REPRESENTATION_CONTEXT ( 3 ) GLOBAL_UNCERTAINTY_ASSIGNED_CONTEXT ( ( #7693 ) ) GLOBAL_UNIT_ASSIGNED_CONTEXT ( ( #2030, #2883, #6966 ) ) REPRESENTATION_CONTEXT ( 'NONE', 'WORKASPACE' ) );
#3811 = DIRECTION ( 'NONE',  ( -0.000000000000000000, -0.000000000000000000, 1.000000000000000000 ) ) ;
#3812 = DIRECTION ( 'NONE',  ( 0.000000000000000000, 0.000000000000000000, 1.000000000000000000 ) ) ;
#3813 = CARTESIAN_POINT ( 'NONE',  ( 0.000000000000000000, 0.000000000000000000, 120.0000000000000142 ) ) ;
#3814 = CONICAL_SURFACE ( 'NONE', #1728, 4.000000000000000000, 0.8911886515913786111 ) ;
#3815 = FACE_OUTER_BOUND ( 'NONE', #1649, .T. ) ;
#3816 = VERTEX_POINT ( 'NONE', #7677 ) ;
#3817 = SURFACE_SIDE_STYLE ('',( #5117 ) ) ;
#3818 = FACE_OUTER_BOUND ( 'NONE', #6390, .T. ) ;
#3819 = ITEM_DEFINED_TRANSFORMATION ( 'NONE', 'NONE', #3232,  #594 ) ;
#3820 = ORIENTED_EDGE ( 'NONE', *, *, #450, .F. ) ;
#3821 = VECTOR ( 'NONE', #4167, 1000.000000000000000 ) ;
#3822 = CARTESIAN_POINT ( 'NONE',  ( 5.000000000000000000, -5.000000000000000000, 148.0000000000000284 ) ) ;
#3823 = VECTOR ( 'NONE', #5932, 1000.000000000000114 ) ;
#3824 = DIRECTION ( 'NONE',  ( -0.000000000000000000, -0.000000000000000000, 1.000000000000000000 ) ) ;
#3825 = CARTESIAN_POINT ( 'NONE',  ( 0.000000000000000000, 0.000000000000000000, -97.99999999999997158 ) ) ;
#3826 = ORIENTED_EDGE ( 'NONE', *, *, #7991, .T. ) ;
#3827 = CARTESIAN_POINT ( 'NONE',  ( -30.00000000000002842, -25.00000000000000000, 200.0000000000000000 ) ) ;
#3828 = DIRECTION ( 'NONE',  ( 0.000000000000000000, 0.000000000000000000, 1.000000000000000000 ) ) ;
#3829 = LINE ( 'NONE', #6476, #156 ) ;
#3830 = ORIENTED_EDGE ( 'NONE', *, *, #7865, .T. ) ;
#3831 = EDGE_LOOP ( 'NONE', ( #7563, #2064, #1704, #6067 ) ) ;
#3832 = EDGE_CURVE ( 'NONE', #6574, #7549, #1712, .T. ) ;
#3833 = DIRECTION ( 'NONE',  ( 1.000000000000000000, 1.734723475976807587E-16, 0.000000000000000000 ) ) ;
#3834 = ADVANCED_FACE ( 'NONE', ( #2369 ), #8332, .F. ) ;
#3835 = DIRECTION ( 'NONE',  ( -1.734723475976807587E-16, 1.000000000000000000, 0.000000000000000000 ) ) ;
#3836 = ADVANCED_FACE ( 'NONE', ( #6357 ), #7012, .T. ) ;
#3837 = CARTESIAN_POINT ( 'NONE',  ( -5.000000000000000000, -5.000000000000000000, 148.0000000000000284 ) ) ;
#3838 = CARTESIAN_POINT ( 'NONE',  ( 1.567478505476134606E-15, 4.618802153517012066, -5.000000000000000000 ) ) ;
#3839 = ORIENTED_EDGE ( 'NONE', *, *, #4580, .T. ) ;
#3840 = FILL_AREA_STYLE ('',( #3185 ) ) ;
#3841 = EDGE_LOOP ( 'NONE', ( #2923, #8157, #4049, #5856 ) ) ;
#3842 = ORIENTED_EDGE ( 'NONE', *, *, #823, .F. ) ;
#3843 = CARTESIAN_POINT ( 'NONE',  ( 2.742827927723449299, 3.035229711104609596, -3.433252694550591233 ) ) ;
#3844 = ADVANCED_FACE ( 'NONE', ( #7990 ), #6094, .F. ) ;
#3845 = AXIS2_PLACEMENT_3D ( 'NONE', #7206, #4637, #3212 ) ;
#3846 = VECTOR ( 'NONE', #3343, 1000.000000000000000 ) ;
#3847 = CARTESIAN_POINT ( 'NONE',  ( -30.00000000000002842, -25.00000000000000000, 200.0000000000000000 ) ) ;
#3848 = PLANE ( 'NONE',  #1954 ) ;
#3849 = DIRECTION ( 'NONE',  ( 0.000000000000000000, 0.000000000000000000, 1.000000000000000000 ) ) ;
#3850 = CARTESIAN_POINT ( 'NONE',  ( 5.000000000000000000, -5.000000000000000000, -0.9999999999999940048 ) ) ;
#3851 = VECTOR ( 'NONE', #2557, 1000.000000000000000 ) ;
#3852 = AXIS2_PLACEMENT_3D ( 'NONE', #4570, #8380, #6451 ) ;
#3853 = LINE ( 'NONE', #1194, #2114 ) ;
#3854 = DIRECTION ( 'NONE',  ( 1.000000000000000000, -1.734723475976806848E-16, 0.000000000000000000 ) ) ;
#3855 = DIRECTION ( 'NONE',  ( -1.734723475976806848E-16, -1.000000000000000000, 0.000000000000000000 ) ) ;
#3856 = EDGE_CURVE ( 'NONE', #2200, #1490, #1361, .T. ) ;
#3857 = DIRECTION ( 'NONE',  ( -0.000000000000000000, 1.000000000000000000, -0.000000000000000000 ) ) ;
#3858 = FACE_OUTER_BOUND ( 'NONE', #1580, .T. ) ;
#3859 = ORIENTED_EDGE ( 'NONE', *, *, #849, .F. ) ;
#3860 = SHAPE_REPRESENTATION_RELATIONSHIP ( 'NONE' , 'NONE' ,  #1533, #7622 ) ;
#3861 = CYLINDRICAL_SURFACE ( 'NONE', #2878, 10.00000000000000000 ) ;
#3862 = CONTEXT_DEPENDENT_SHAPE_REPRESENTATION ( #2702, #1716 ) ;
#3863 = EDGE_LOOP ( 'NONE', ( #1393, #2329, #3463, #909 ) ) ;
#3864 = CARTESIAN_POINT ( 'NONE',  ( 107.9310344827585908, -20.00000000000000000, -144.8275862068965125 ) ) ;
#3865 = EDGE_CURVE ( 'NONE', #2200, #8282, #8077, .T. ) ;
#3866 = CARTESIAN_POINT ( 'NONE',  ( 434.9999999999999432, -4.999999999999998224, 140.0000000000000000 ) ) ;
#3867 = ADVANCED_FACE ( 'NONE', ( #5364 ), #7370, .F. ) ;
#3868 = PRESENTATION_LAYER_ASSIGNMENT (  '', '', ( #6917 ) ) ;
#3869 = PLANE ( 'NONE',  #3552 ) ;
#3870 = EDGE_LOOP ( 'NONE', ( #4110, #5610, #908, #3052, #857 ) ) ;
#3871 = LINE ( 'NONE', #3827, #6009 ) ;
#3872 = APPLICATION_PROTOCOL_DEFINITION ( 'draft international standard', 'automotive_design', 1998, #179 ) ;
#3873 = DIRECTION ( 'NONE',  ( 1.000000000000000000, 0.000000000000000000, 0.000000000000000000 ) ) ;
#3874 = ORIENTED_EDGE ( 'NONE', *, *, #6909, .T. ) ;
#3875 = ORIENTED_EDGE ( 'NONE', *, *, #8572, .T. ) ;
#3876 = CARTESIAN_POINT ( 'NONE',  ( 0.000000000000000000, 0.000000000000000000, -43.99999999999997158 ) ) ;
#3877 = FACE_OUTER_BOUND ( 'NONE', #6525, .T. ) ;
#3878 = CARTESIAN_POINT ( 'NONE',  ( -10.00000000000000000, 1.224646799147353256E-15, 120.0000000000000142 ) ) ;
#3879 = ADVANCED_FACE ( 'NONE', ( #4107 ), #3283, .F. ) ;
#3880 = AXIS2_PLACEMENT_3D ( 'NONE', #4403, #7053, #6446 ) ;
#3881 = CARTESIAN_POINT ( 'NONE',  ( 5.000000000000000000, -5.000000000000000000, 140.0000000000000000 ) ) ;
#3882 = VERTEX_POINT ( 'NONE', #762 ) ;
#3883 = ORIENTED_EDGE ( 'NONE', *, *, #7246, .T. ) ;
#3884 = CARTESIAN_POINT ( 'NONE',  ( 0.000000000000000000, 0.000000000000000000, 148.0000000000000284 ) ) ;
#3885 = CIRCLE ( 'NONE', #8341, 2.649999999999985700 ) ;
#3886 = B_SPLINE_CURVE_WITH_KNOTS ( 'NONE', 3,
 ( #2487, #4511, #1873, #3085, #8318, #8449 ),
 .UNSPECIFIED., .F., .F.,
 ( 4, 2, 4 ),
 ( 0.003358874760055550156, 0.004541967308452096383, 0.005725059856848641743 ),
 .UNSPECIFIED. ) ;
#3887 = FACE_OUTER_BOUND ( 'NONE', #3027, .T. ) ;
#3888 = LINE ( 'NONE', #1354, #8042 ) ;
#3889 = FACE_OUTER_BOUND ( 'NONE', #6715, .T. ) ;
#3890 = SURFACE_STYLE_FILL_AREA ( #8471 ) ;
#3891 = AXIS2_PLACEMENT_3D ( 'NONE', #6495, #534, #3195 ) ;
#3892 = CARTESIAN_POINT ( 'NONE',  ( 259.0000000000000000, 5.000000000000001776, 145.0000000000000284 ) ) ;
#3893 = LINE ( 'NONE', #1196, #6021 ) ;
#3894 = DIRECTION ( 'NONE',  ( -1.734723475976807587E-16, 1.000000000000000000, 0.000000000000000000 ) ) ;
#3895 = AXIS2_PLACEMENT_3D ( 'NONE', #7501, #1018, #2197 ) ;
#3896 = DIRECTION ( 'NONE',  ( 0.000000000000000000, 0.000000000000000000, 1.000000000000000000 ) ) ;
#3897 = LINE ( 'NONE', #2594, #1485 ) ;
#3898 = ORIENTED_EDGE ( 'NONE', *, *, #1735, .T. ) ;
#3899 = CARTESIAN_POINT ( 'NONE',  ( -2.000000000000006661, 3.464101615137750834, 0.000000000000000000 ) ) ;
#3900 = ITEM_DEFINED_TRANSFORMATION ( 'NONE', 'NONE', #5989,  #594 ) ;
#3901 = ORIENTED_EDGE ( 'NONE', *, *, #6636, .T. ) ;
#3902 = CARTESIAN_POINT ( 'NONE',  ( 3.333333333333332593, 2.694301256218250007, -3.300726591567078483 ) ) ;
#3903 = CARTESIAN_POINT ( 'NONE',  ( -5.000000000000000000, -5.000000000000000000, -105.9999999999999858 ) ) ;
#3904 = ADVANCED_FACE ( 'NONE', ( #1450 ), #7233, .F. ) ;
#3905 = CARTESIAN_POINT ( 'NONE',  ( 0.000000000000000000, 0.000000000000000000, 200.0000000000000000 ) ) ;
#3906 = ADVANCED_FACE ( 'NONE', ( #803 ), #550, .F. ) ;
#3907 = EDGE_LOOP ( 'NONE', ( #4374, #2568 ) ) ;
#3908 = CARTESIAN_POINT ( 'NONE',  ( -10.00000000000000000, 1.224646799147353256E-15, 42.00000000000000711 ) ) ;
#3909 = DIRECTION ( 'NONE',  ( 0.9647346005781386458, -1.387778780781445676E-17, 0.2632245247831960233 ) ) ;
#3910 = CARTESIAN_POINT ( 'NONE',  ( -4.999999999999998224, 134.9989999999999952, 15.00000000000000355 ) ) ;
#3911 = ORIENTED_EDGE ( 'NONE', *, *, #5222, .F. ) ;
#3912 = ADVANCED_FACE ( 'NONE', ( #6625 ), #4581, .F. ) ;
#3913 = VERTEX_POINT ( 'NONE', #7898 ) ;
#3914 =( GEOMETRIC_REPRESENTATION_CONTEXT ( 3 ) GLOBAL_UNCERTAINTY_ASSIGNED_CONTEXT ( ( #4377 ) ) GLOBAL_UNIT_ASSIGNED_CONTEXT ( ( #115, #8191, #6872 ) ) REPRESENTATION_CONTEXT ( 'NONE', 'WORKASPACE' ) );
#3915 = DIRECTION ( 'NONE',  ( -1.000000000000000000, 0.000000000000000000, 0.000000000000000000 ) ) ;
#3916 = PLANE ( 'NONE',  #1038 ) ;
#3917 = APPLICATION_CONTEXT ( 'automotive_design' ) ;
#3918 = CARTESIAN_POINT ( 'NONE',  ( 4.000000000000000000, -1.677850389431204459, -3.535268758346977513 ) ) ;
#3919 = AXIS2_PLACEMENT_3D ( 'NONE', #3050, #1829, #7130 ) ;
#3920 = PRODUCT ( 'roller axis assy_r4', 'roller axis assy_r4', '', ( #3259 ) ) ;
#3921 = DIRECTION ( 'NONE',  ( -0.000000000000000000, 1.000000000000000000, -0.000000000000000000 ) ) ;
#3922 = ORIENTED_EDGE ( 'NONE', *, *, #5547, .T. ) ;
#3923 = VERTEX_POINT ( 'NONE', #7414 ) ;
#3924 = LINE ( 'NONE', #1225, #1151 ) ;
#3925 = EDGE_CURVE ( 'NONE', #5594, #3511, #5414, .T. ) ;
#3926 = PRESENTATION_LAYER_ASSIGNMENT (  '', '', ( #581 ) ) ;
#3927 = FACE_OUTER_BOUND ( 'NONE', #6670, .T. ) ;
#3928 = CARTESIAN_POINT ( 'NONE',  ( 5.000000000000000000, 5.000000000000000000, 148.0000000000000284 ) ) ;
#3929 = ORIENTED_EDGE ( 'NONE', *, *, #5472, .T. ) ;
#3930 = CARTESIAN_POINT ( 'NONE',  ( 5.000000000000000000, -5.000000000000000000, -143.0000000000000284 ) ) ;
#3931 =( LENGTH_UNIT ( ) NAMED_UNIT ( * ) SI_UNIT ( .MILLI., .METRE. ) );
#3932 = CONICAL_SURFACE ( 'NONE', #163, 2.055000000000000160, 0.7853981633974721488 ) ;
#3933 = UNCERTAINTY_MEASURE_WITH_UNIT (LENGTH_MEASURE( 1.000000000000000082E-05 ), #6030, 'distance_accuracy_value', 'NONE');
#3934 = VECTOR ( 'NONE', #174, 1000.000000000000000 ) ;
#3935 = CARTESIAN_POINT ( 'NONE',  ( -5.000000000000001776, 5.000000000000001776, 148.0000000000000284 ) ) ;
#3936 = AXIS2_PLACEMENT_3D ( 'NONE', #5811, #2525, #1875 ) ;
#3937 = CARTESIAN_POINT ( 'NONE',  ( 470.0000000000000000, -25.00000000000000000, 200.0000000000000000 ) ) ;
#3938 = EDGE_CURVE ( 'NONE', #3209, #7011, #7942, .T. ) ;
#3939 = ADVANCED_FACE ( 'NONE', ( #4064, #5925 ), #6708, .T. ) ;
#3940 = CARTESIAN_POINT ( 'NONE',  ( -5.000000000000001776, 5.000000000000001776, -143.0000000000000284 ) ) ;
#3941 = VECTOR ( 'NONE', #2059, 1000.000000000000000 ) ;
#3942 = ADVANCED_FACE ( 'NONE', ( #3412, #624 ), #8599, .T. ) ;
#3943 = DIRECTION ( 'NONE',  ( -1.000000000000000000, 0.000000000000000000, 0.000000000000000000 ) ) ;
#3944 = VECTOR ( 'NONE', #2908, 1000.000000000000000 ) ;
#3945 = LINE ( 'NONE', #7196, #2907 ) ;
#3946 = LINE ( 'NONE', #6586, #7604 ) ;
#3947 = ORIENTED_EDGE ( 'NONE', *, *, #67, .T. ) ;
#3948 = FACE_OUTER_BOUND ( 'NONE', #915, .T. ) ;
#3949 = ITEM_DEFINED_TRANSFORMATION ( 'NONE', 'NONE', #8510,  #594 ) ;
#3950 = ORIENTED_EDGE ( 'NONE', *, *, #7126, .T. ) ;
#3951 = CARTESIAN_POINT ( 'NONE',  ( -20.00000000000000000, 140.0000000000000000, 5.000000000000000000 ) ) ;
#3952 = CARTESIAN_POINT ( 'NONE',  ( 1.654252653721905331, 3.663718938583014229, -0.01223254789873410957 ) ) ;
#3953 = CIRCLE ( 'NONE', #7569, 2.649999999999985700 ) ;
#3954 = PRODUCT_DEFINITION_CONTEXT ( 'detailed design', #2251, 'design' ) ;
#3955 = B_SPLINE_CURVE_WITH_KNOTS ( 'NONE', 3,
 ( #6826, #2874, #8192, #8150 ),
 .UNSPECIFIED., .F., .F.,
 ( 4, 4 ),
 ( 0.000000000000000000, 0.002452478801916376308 ),
 .UNSPECIFIED. ) ;
#3956 = CARTESIAN_POINT ( 'NONE',  ( 4.000000000000000000, 2.309401076758497151, -5.000000000000000000 ) ) ;
#3957 = ORIENTED_EDGE ( 'NONE', *, *, #3802, .T. ) ;
#3958 = DIRECTION ( 'NONE',  ( -0.000000000000000000, 1.000000000000000000, -0.000000000000000000 ) ) ;
#3959 = CIRCLE ( 'NONE', #8416, 2.649999999999985700 ) ;
#3960 = APPLICATION_PROTOCOL_DEFINITION ( 'draft international standard', 'automotive_design', 1998, #6861 ) ;
#3961 = CARTESIAN_POINT ( 'NONE',  ( -5.000000000000000000, -5.000000000000000000, -71.99999999999998579 ) ) ;
#3962 = ORIENTED_EDGE ( 'NONE', *, *, #3006, .T. ) ;
#3963 = ORIENTED_EDGE ( 'NONE', *, *, #8547, .F. ) ;
#3964 = CARTESIAN_POINT ( 'NONE',  ( 5.000000000000000000, 5.000000000000000000, 34.00000000000000711 ) ) ;
#3965 = DIRECTION ( 'NONE',  ( 1.000000000000000000, 0.000000000000000000, 0.000000000000000000 ) ) ;
#3966 = EDGE_CURVE ( 'NONE', #7425, #3298, #2632, .T. ) ;
#3967 = CARTESIAN_POINT ( 'NONE',  ( 4.000000000000000000, -2.511475576507276042, -3.469253905236643565 ) ) ;
#3968 = CARTESIAN_POINT ( 'NONE',  ( 170.9999999999999716, -4.999999999999998224, 139.9990000000000236 ) ) ;
#3969 = ORIENTED_EDGE ( 'NONE', *, *, #1653, .F. ) ;
#3970 = FILL_AREA_STYLE_COLOUR ( '', #4051 ) ;
#3971 = ORIENTED_EDGE ( 'NONE', *, *, #5195, .T. ) ;
#3972 = CARTESIAN_POINT ( 'NONE',  ( 20.00000000000000000, 0.000000000000000000, -120.5685424949237898 ) ) ;
#3973 = VECTOR ( 'NONE', #6077, 1000.000000000000000 ) ;
#3974 = CARTESIAN_POINT ( 'NONE',  ( 347.0000000000000000, 5.000000000000001776, 140.0000000000000000 ) ) ;
#3975 = DIRECTION ( 'NONE',  ( 1.000000000000000000, 0.000000000000000000, 0.000000000000000000 ) ) ;
#3976 = VERTEX_POINT ( 'NONE', #6054 ) ;
#3977 = DIRECTION ( 'NONE',  ( -1.734723475976807587E-16, 1.000000000000000000, 0.000000000000000000 ) ) ;
#3978 = LINE ( 'NONE', #667, #1427 ) ;
#3979 = ADVANCED_BREP_SHAPE_REPRESENTATION ( '', ( #1986, #594 ), #1408 ) ;
#3980 = CIRCLE ( 'NONE', #2470, 2.649999999999985700 ) ;
#3981 = CARTESIAN_POINT ( 'NONE',  ( -10.00000000000000000, 1.224646799147353256E-15, 7.000000000000006217 ) ) ;
#3982 = LINE ( 'NONE', #7158, #1281 ) ;
#3983 = DIRECTION ( 'NONE',  ( 0.000000000000000000, 0.000000000000000000, 1.000000000000000000 ) ) ;
#3984 = CARTESIAN_POINT ( 'NONE',  ( -5.000000000000000000, -5.000000000000000000, 140.0000000000000000 ) ) ;
#3985 = CARTESIAN_POINT ( 'NONE',  ( 269.0000000000000000, 5.000000000000000000, 139.9990000000000236 ) ) ;
#3986 = EDGE_CURVE ( 'NONE', #5212, #7983, #7328, .T. ) ;
#3987 = CLOSED_SHELL ( 'NONE', ( #4357, #1181, #4197, #1665, #57, #512, #3696, #393, #3610, #5701, #3912, #6378, #5921, #5566 ) ) ;
#3988 = ORIENTED_EDGE ( 'NONE', *, *, #4865, .F. ) ;
#3989 = EDGE_CURVE ( 'NONE', #2349, #6369, #2887, .T. ) ;
#3990 = ORIENTED_EDGE ( 'NONE', *, *, #8090, .T. ) ;
#3991 = CONTEXT_DEPENDENT_SHAPE_REPRESENTATION ( #4519, #7694 ) ;
#3992 = EDGE_LOOP ( 'NONE', ( #1461, #3749, #371, #6989 ) ) ;
#3993 = CARTESIAN_POINT ( 'NONE',  ( 0.2500000000000002220, 4.898587196589412829E-16, -4.000000000000000000 ) ) ;
#3994 = PLANE ( 'NONE',  #1296 ) ;
#3995 = AXIS2_PLACEMENT_3D ( 'NONE', #495, #4494, #1894 ) ;
#3996 = PRODUCT_DEFINITION_SHAPE ( 'NONE', 'NONE',  #424 ) ;
#3997 = CARTESIAN_POINT ( 'NONE',  ( 2.500000000000000000, 2.357898499370433054, -1.951563910473907981E-15 ) ) ;
#3998 = ORIENTED_EDGE ( 'NONE', *, *, #3635, .T. ) ;
#3999 = CARTESIAN_POINT ( 'NONE',  ( 4.211140560182196957, 2.431303136016536470, -3.745885042887433514 ) ) ;
#4000 = PLANE ( 'NONE',  #1203 ) ;
#4001 = CARTESIAN_POINT ( 'NONE',  ( 440.0000000000000000, -10.00000000000001243, 18.96857495968452767 ) ) ;
#4002 = FACE_BOUND ( 'NONE', #722, .T. ) ;
#4003 = ORIENTED_EDGE ( 'NONE', *, *, #7571, .T. ) ;
#4004 = EDGE_LOOP ( 'NONE', ( #4516, #3950, #1386, #4946 ) ) ;
#4005 = CARTESIAN_POINT ( 'NONE',  ( -4.999999999999998224, 134.9989999999999952, 15.00000000000000355 ) ) ;
#4006 = DIRECTION ( 'NONE',  ( -1.734723475976807587E-16, 1.000000000000000000, 0.000000000000000000 ) ) ;
#4007 = CARTESIAN_POINT ( 'NONE',  ( 4.000000000000000000, 2.309401076758497151, -5.000000000000000000 ) ) ;
#4008 = DIRECTION ( 'NONE',  ( 1.000000000000000000, 0.000000000000000000, 0.000000000000000000 ) ) ;
#4009 = ORIENTED_EDGE ( 'NONE', *, *, #3222, .F. ) ;
#4010 = VERTEX_POINT ( 'NONE', #4322 ) ;
#4011 = CARTESIAN_POINT ( 'NONE',  ( 0.1404048886732821022, 4.699864953788070565, -3.686887068327037387 ) ) ;
#4012 = AXIS2_PLACEMENT_3D ( 'NONE', #7844, #8018, #2011 ) ;
#4013 = CARTESIAN_POINT ( 'NONE',  ( -20.00000000000000000, 2.449293598294706513E-15, 120.0000000000000142 ) ) ;
#4014 = ADVANCED_FACE ( 'NONE', ( #129 ), #5623, .T. ) ;
#4015 = LINE ( 'NONE', #3359, #1223 ) ;
#4016 = ORIENTED_EDGE ( 'NONE', *, *, #5750, .F. ) ;
#4017 = DIRECTION ( 'NONE',  ( -0.000000000000000000, -0.000000000000000000, -1.000000000000000000 ) ) ;
#4018 = ADVANCED_FACE ( 'NONE', ( #180 ), #2645, .F. ) ;
#4019 = CIRCLE ( 'NONE', #1803, 2.649999999999985700 ) ;
#4020 = EDGE_CURVE ( 'NONE', #7663, #7048, #5494, .T. ) ;
#4021 = CARTESIAN_POINT ( 'NONE',  ( -10.00000000000000000, 1.224646799147353256E-15, 140.0000000000000000 ) ) ;
#4022 = DIRECTION ( 'NONE',  ( -0.000000000000000000, -0.000000000000000000, 1.000000000000000000 ) ) ;
#4023 = AXIS2_PLACEMENT_3D ( 'NONE', #6182, #6792, #1535 ) ;
#4024 = DIRECTION ( 'NONE',  ( 1.000000000000000000, 0.000000000000000000, 0.000000000000000000 ) ) ;
#4025 = CARTESIAN_POINT ( 'NONE',  ( -5.000000000000000000, -5.000000000000000000, 7.000000000000006217 ) ) ;
#4026 = FACE_OUTER_BOUND ( 'NONE', #7511, .T. ) ;
#4027 = EDGE_LOOP ( 'NONE', ( #2212, #6146, #2282, #5992 ) ) ;
#4028 = VERTEX_POINT ( 'NONE', #2930 ) ;
#4029 = ORIENTED_EDGE ( 'NONE', *, *, #7307, .T. ) ;
#4030 = CARTESIAN_POINT ( 'NONE',  ( 10.00000000000000000, 0.000000000000000000, 140.0000000000000000 ) ) ;
#4031 = AXIS2_PLACEMENT_3D ( 'NONE', #7019, #5187, #355 ) ;
#4032 = CARTESIAN_POINT ( 'NONE',  ( 5.000000000000001776, 135.0000000000000000, 15.00000000000000355 ) ) ;
#4033 = EDGE_CURVE ( 'NONE', #3807, #7646, #6142, .T. ) ;
#4034 = ORIENTED_EDGE ( 'NONE', *, *, #7283, .F. ) ;
#4035 = CARTESIAN_POINT ( 'NONE',  ( 20.00000000000000000, 0.000000000000000000, -77.99999999999997158 ) ) ;
#4036 = CIRCLE ( 'NONE', #2234, 2.100000000000000089 ) ;
#4037 = EDGE_LOOP ( 'NONE', ( #2293, #2094, #5778, #3314 ) ) ;
#4038 = CARTESIAN_POINT ( 'NONE',  ( -10.00000000000000000, 1.224646799147353059E-15, 120.0000000000000284 ) ) ;
#4039 = DIRECTION ( 'NONE',  ( 1.000000000000000000, 0.000000000000000000, 0.000000000000000000 ) ) ;
#4040 = DIRECTION ( 'NONE',  ( -1.040834085586084257E-17, -0.9999999999999998890, -5.551115123125782702E-17 ) ) ;
#4041 = SURFACE_SIDE_STYLE ('',( #2166 ) ) ;
#4042 = ORIENTED_EDGE ( 'NONE', *, *, #939, .F. ) ;
#4043 = ORIENTED_EDGE ( 'NONE', *, *, #1504, .F. ) ;
#4044 = DIRECTION ( 'NONE',  ( -1.000000000000000000, 0.000000000000000000, 0.000000000000000000 ) ) ;
#4045 = CARTESIAN_POINT ( 'NONE',  ( 181.0000000000000000, -4.999999999999998224, 139.9990000000000236 ) ) ;
#4046 = DIRECTION ( 'NONE',  ( -1.000000000000000000, 1.734723475976807587E-16, 0.000000000000000000 ) ) ;
#4047 = FACE_OUTER_BOUND ( 'NONE', #4078, .T. ) ;
#4048 = ORIENTED_EDGE ( 'NONE', *, *, #3433, .F. ) ;
#4049 = ORIENTED_EDGE ( 'NONE', *, *, #2296, .F. ) ;
#4050 = CARTESIAN_POINT ( 'NONE',  ( -0.5276280594146446346, 4.314175951381965746, -3.320322319201721495 ) ) ;
#4051 = COLOUR_RGB ( '',0.8941176470588234615, 0.8941176470588234615, 0.8941176470588234615 ) ;
#4052 = DIRECTION ( 'NONE',  ( -0.000000000000000000, 1.000000000000000000, -0.000000000000000000 ) ) ;
#4053 = CARTESIAN_POINT ( 'NONE',  ( 93.00000000000000000, 5.000000000000000000, 140.0000000000000000 ) ) ;
#4054 = ORIENTED_EDGE ( 'NONE', *, *, #6383, .F. ) ;
#4055 = CARTESIAN_POINT ( 'NONE',  ( 386.6666666666666288, -20.00000000000000000, 162.5000000000000853 ) ) ;
#4056 = ORIENTED_EDGE ( 'NONE', *, *, #4975, .F. ) ;
#4057 = PRODUCT_DEFINITION_SHAPE ( 'NONE', 'NONE',  #8605 ) ;
#4058 = DIRECTION ( 'NONE',  ( 0.000000000000000000, 0.000000000000000000, -1.000000000000000000 ) ) ;
#4059 = EDGE_CURVE ( 'NONE', #5369, #8255, #2978, .T. ) ;
#4060 = CYLINDRICAL_SURFACE ( 'NONE', #3366, 2.649999999999985700 ) ;
#4061 = AXIS2_PLACEMENT_3D ( 'NONE', #538, #4578, #7232 ) ;
#4062 = ADVANCED_FACE ( 'NONE', ( #8297 ), #3674, .T. ) ;
#4063 = DIRECTION ( 'NONE',  ( -0.000000000000000000, -0.000000000000000000, 1.000000000000000000 ) ) ;
#4064 = FACE_BOUND ( 'NONE', #6863, .T. ) ;
#4065 = AXIS2_PLACEMENT_3D ( 'NONE', #6580, #4058, #8596 ) ;
#4066 = ADVANCED_FACE ( 'NONE', ( #4801 ), #975, .F. ) ;
#4067 = DIRECTION ( 'NONE',  ( -1.000000000000000000, 0.000000000000000000, 0.000000000000000000 ) ) ;
#4068 = DIRECTION ( 'NONE',  ( -1.000000000000000000, 0.000000000000000000, 0.000000000000000000 ) ) ;
#4069 = EDGE_LOOP ( 'NONE', ( #3026, #3962, #1775, #5163 ) ) ;
#4070 = ORIENTED_EDGE ( 'NONE', *, *, #8432, .T. ) ;
#4071 = UNCERTAINTY_MEASURE_WITH_UNIT (LENGTH_MEASURE( 1.000000000000000082E-05 ), #2770, 'distance_accuracy_value', 'NONE');
#4072 = ORIENTED_EDGE ( 'NONE', *, *, #5998, .F. ) ;
#4073 = CARTESIAN_POINT ( 'NONE',  ( -10.00000000000000000, 1.224646799147353059E-15, -7.999999999999996447 ) ) ;
#4074 = CIRCLE ( 'NONE', #8252, 2.649999999999985700 ) ;
#4075 = FACE_OUTER_BOUND ( 'NONE', #7527, .T. ) ;
#4076 = VECTOR ( 'NONE', #6806, 1000.000000000000000 ) ;
#4077 =( GEOMETRIC_REPRESENTATION_CONTEXT ( 3 ) GLOBAL_UNCERTAINTY_ASSIGNED_CONTEXT ( ( #1069 ) ) GLOBAL_UNIT_ASSIGNED_CONTEXT ( ( #4318, #2235, #6228 ) ) REPRESENTATION_CONTEXT ( 'NONE', 'WORKASPACE' ) );
#4078 = EDGE_LOOP ( 'NONE', ( #778, #3654, #3688, #3086, #3729, #3957, #6902 ) ) ;
#4079 = DIRECTION ( 'NONE',  ( -0.000000000000000000, -0.000000000000000000, -1.000000000000000000 ) ) ;
#4080 = ORIENTED_EDGE ( 'NONE', *, *, #288, .T. ) ;
#4081 = DIRECTION ( 'NONE',  ( -1.000000000000000000, -0.000000000000000000, -0.000000000000000000 ) ) ;
#4082 =( REPRESENTATION_RELATIONSHIP ('NONE','NONE', #3312, #4754 ) REPRESENTATION_RELATIONSHIP_WITH_TRANSFORMATION ( #3949 )SHAPE_REPRESENTATION_RELATIONSHIP( ) );
#4083 = CARTESIAN_POINT ( 'NONE',  ( 470.0000000000000000, -19.99999999999979394, 0.000000000000000000 ) ) ;
#4084 = ITEM_DEFINED_TRANSFORMATION ( 'NONE', 'NONE', #6962,  #594 ) ;
#4085 =( NAMED_UNIT ( * ) SI_UNIT ( $, .STERADIAN. ) SOLID_ANGLE_UNIT ( ) );
#4086 = ORIENTED_EDGE ( 'NONE', *, *, #4538, .F. ) ;
#4087 = CIRCLE ( 'NONE', #1583, 4.000000000000000000 ) ;
#4088 = ORIENTED_EDGE ( 'NONE', *, *, #1168, .F. ) ;
#4089 = VECTOR ( 'NONE', #8260, 1000.000000000000000 ) ;
#4090 = LINE ( 'NONE', #8229, #6703 ) ;
#4091 = CARTESIAN_POINT ( 'NONE',  ( -2.500000000000000888, 0.000000000000000000, -4.974599999999998801 ) ) ;
#4092 = AXIS2_PLACEMENT_3D ( 'NONE', #483, #7797, #4479 ) ;
#4093 = CARTESIAN_POINT ( 'NONE',  ( 4.000000000000000000, -1.700175430507292473, -3.320327275037661785 ) ) ;
#4094 = CARTESIAN_POINT ( 'NONE',  ( -4.000000000000000000, -2.309401076758512694, -5.000000000000000000 ) ) ;
#4095 = ORIENTED_EDGE ( 'NONE', *, *, #3159, .T. ) ;
#4096 = EDGE_CURVE ( 'NONE', #3374, #3298, #8209, .T. ) ;
#4097 = DIRECTION ( 'NONE',  ( 0.000000000000000000, 0.000000000000000000, -1.000000000000000000 ) ) ;
#4098 = ORIENTED_EDGE ( 'NONE', *, *, #2229, .T. ) ;
#4099 = EDGE_CURVE ( 'NONE', #5237, #3653, #889, .T. ) ;
#4100 = ORIENTED_EDGE ( 'NONE', *, *, #2927, .T. ) ;
#4101 = CARTESIAN_POINT ( 'NONE',  ( -2.171643655288372443, 3.365003104552320767, 2.541098841762897165E-18 ) ) ;
#4102 = CARTESIAN_POINT ( 'NONE',  ( -5.000000000000000000, -5.000000000000000000, -71.99999999999998579 ) ) ;
#4103 = DIRECTION ( 'NONE',  ( -1.000000000000000000, 0.000000000000000000, 0.000000000000000000 ) ) ;
#4104 = ORIENTED_EDGE ( 'NONE', *, *, #2742, .F. ) ;
#4105 = CARTESIAN_POINT ( 'NONE',  ( 0.000000000000000000, 0.000000000000000000, 120.0000000000000142 ) ) ;
#4106 = DIRECTION ( 'NONE',  ( -1.734723475976806848E-16, 1.000000000000000000, 0.000000000000000000 ) ) ;
#4107 = FACE_OUTER_BOUND ( 'NONE', #2596, .T. ) ;
#4108 = DIRECTION ( 'NONE',  ( -0.000000000000000000, 1.000000000000000000, -0.000000000000000000 ) ) ;
#4109 = DIRECTION ( 'NONE',  ( -1.734723475976807341E-16, 1.000000000000000000, 0.000000000000000000 ) ) ;
#4110 = ORIENTED_EDGE ( 'NONE', *, *, #7218, .T. ) ;
#4111 = VECTOR ( 'NONE', #8370, 1000.000000000000000 ) ;
#4112 = ORIENTED_EDGE ( 'NONE', *, *, #2524, .T. ) ;
#4113 = CLOSED_SHELL ( 'NONE', ( #742, #1429, #7592, #3867, #4925, #1058, #6100, #6266, #4811, #3904, #8106, #557, #6660, #439, #4440, #1570, #4694, #8286, #7151, #5556, #1169, #397, #3660, #4437, #1864, #2660, #8014, #6028 ) ) ;
#4114 = EDGE_LOOP ( 'NONE', ( #7237, #4296, #5435, #1724 ) ) ;
#4115 = DIRECTION ( 'NONE',  ( -0.000000000000000000, 1.000000000000000000, -0.000000000000000000 ) ) ;
#4116 = CONICAL_SURFACE ( 'NONE', #7039, 4.000000000000000000, 0.8911886515913786111 ) ;
#4117 = ORIENTED_EDGE ( 'NONE', *, *, #6034, .T. ) ;
#4118 = DIRECTION ( 'NONE',  ( -0.000000000000000000, 0.000000000000000000, 1.000000000000000000 ) ) ;
#4119 = ORIENTED_EDGE ( 'NONE', *, *, #4580, .F. ) ;
#4120 = FACE_BOUND ( 'NONE', #5672, .T. ) ;
#4121 = CARTESIAN_POINT ( 'NONE',  ( 0.000000000000000000, 0.000000000000000000, -43.99999999999997158 ) ) ;
#4122 = EDGE_CURVE ( 'NONE', #1609, #4392, #5574, .T. ) ;
#4123 = DIRECTION ( 'NONE',  ( -1.000000000000000000, 0.000000000000000000, -0.000000000000000000 ) ) ;
#4124 = EDGE_LOOP ( 'NONE', ( #5871, #1590, #676, #5723 ) ) ;
#4125 = ORIENTED_EDGE ( 'NONE', *, *, #5998, .T. ) ;
#4126 = VECTOR ( 'NONE', #4109, 1000.000000000000000 ) ;
#4128 = VECTOR ( 'NONE', #4747, 1000.000000000000000 ) ;
#4127 = DIRECTION ( 'NONE',  ( 0.000000000000000000, 0.000000000000000000, -1.000000000000000000 ) ) ;
#4129 = ADVANCED_FACE ( 'NONE', ( #6232 ), #3067, .F. ) ;
#4130 = DIRECTION ( 'NONE',  ( 0.000000000000000000, 0.000000000000000000, 1.000000000000000000 ) ) ;
#4131 = CARTESIAN_POINT ( 'NONE',  ( -3.861362476283256129, -2.629030857716004199, -3.671615880910374941 ) ) ;
#4132 = PRODUCT_DEFINITION_SHAPE ( 'NONE', 'NONE',  #3780 ) ;
#4133 = FACE_OUTER_BOUND ( 'NONE', #506, .T. ) ;
#4134 = VERTEX_POINT ( 'NONE', #2238 ) ;
#4135 = FACE_OUTER_BOUND ( 'NONE', #3360, .T. ) ;
#4136 = ORIENTED_EDGE ( 'NONE', *, *, #306, .F. ) ;
#4137 = ORIENTED_EDGE ( 'NONE', *, *, #6722, .F. ) ;
#4138 = CARTESIAN_POINT ( 'NONE',  ( 0.000000000000000000, 0.000000000000000000, -77.99999999999997158 ) ) ;
#4139 = EDGE_CURVE ( 'NONE', #4673, #7074, #8123, .T. ) ;
#4140 = DIRECTION ( 'NONE',  ( -0.000000000000000000, -0.000000000000000000, 1.000000000000000000 ) ) ;
#4141 = CARTESIAN_POINT ( 'NONE',  ( 1.567478505476134606E-15, 4.618802153517012066, -5.000000000000000000 ) ) ;
#4142 = EDGE_LOOP ( 'NONE', ( #106, #3227, #4486, #7679 ) ) ;
#4143 = CARTESIAN_POINT ( 'NONE',  ( 5.000000000000000000, 5.000000000000000000, 42.00000000000000711 ) ) ;
#4144 = DIRECTION ( 'NONE',  ( 0.000000000000000000, 0.000000000000000000, 1.000000000000000000 ) ) ;
#4145 = LINE ( 'NONE', #760, #3647 ) ;
#4146 = DIRECTION ( 'NONE',  ( 0.000000000000000000, 0.000000000000000000, 1.000000000000000000 ) ) ;
#4147 = CARTESIAN_POINT ( 'NONE',  ( 5.000000000000000000, 5.000000000000000000, -105.9999999999999858 ) ) ;
#4148 = DIRECTION ( 'NONE',  ( 0.000000000000000000, 0.000000000000000000, 1.000000000000000000 ) ) ;
#4149 = AXIS2_PLACEMENT_3D ( 'NONE', #3579, #2189, #123 ) ;
#4150 = EDGE_LOOP ( 'NONE', ( #3790, #8372 ) ) ;
#4151 = ORIENTED_EDGE ( 'NONE', *, *, #202, .F. ) ;
#4152 = EDGE_LOOP ( 'NONE', ( #5280, #1640, #7829, #5540 ) ) ;
#4153 = DIRECTION ( 'NONE',  ( -0.000000000000000000, -0.000000000000000000, 1.000000000000000000 ) ) ;
#4154 = CIRCLE ( 'NONE', #7209, 2.041999999999999815 ) ;
#4155 = EDGE_LOOP ( 'NONE', ( #8128, #2305, #4882, #6504 ) ) ;
#4156 = DIRECTION ( 'NONE',  ( -1.000000000000000000, 1.224646799147352714E-16, 0.000000000000000000 ) ) ;
#4157 = ORIENTED_EDGE ( 'NONE', *, *, #6430, .F. ) ;
#4158 = PLANE ( 'NONE',  #7973 ) ;
#4159 = B_SPLINE_CURVE_WITH_KNOTS ( 'NONE', 3,
 ( #5193, #2024, #8509, #7282, #623, #3243 ),
 .UNSPECIFIED., .F., .F.,
 ( 4, 2, 4 ),
 ( 4.336808689942017736E-19, 0.0002095117440854729585, 0.0004190234881709454834 ),
 .UNSPECIFIED. ) ;
#4160 = CARTESIAN_POINT ( 'NONE',  ( 0.000000000000000000, 0.000000000000000000, -154.5685424949238040 ) ) ;
#4161 = VECTOR ( 'NONE', #2239, 1000.000000000000000 ) ;
#4162 = PRODUCT_CONTEXT ( 'NONE', #9, 'mechanical' ) ;
#4163 = CARTESIAN_POINT ( 'NONE',  ( 470.0000000000000000, -20.00000000000000000, 180.0000000000000284 ) ) ;
#4164 = VERTEX_POINT ( 'NONE', #7595 ) ;
#4165 = ORIENTED_EDGE ( 'NONE', *, *, #6239, .T. ) ;
#4166 = CARTESIAN_POINT ( 'NONE',  ( -5.000000000000000000, -5.000000000000000000, -27.99999999999999645 ) ) ;
#4167 = DIRECTION ( 'NONE',  ( -1.000000000000000000, 1.734723475976807587E-16, 0.000000000000000000 ) ) ;
#4168 = EDGE_CURVE ( 'NONE', #8492, #1599, #4279, .T. ) ;
#4169 = ADVANCED_FACE ( 'NONE', ( #4888 ), #1497, .T. ) ;
#4170 = CARTESIAN_POINT ( 'NONE',  ( -30.00000000000002842, -25.00000000000000000, -200.0000000000000000 ) ) ;
#4171 = CARTESIAN_POINT ( 'NONE',  ( 0.5276280594147412240, -4.314175951381924889, -3.320322319201654881 ) ) ;
#4172 = ORIENTED_EDGE ( 'NONE', *, *, #2311, .F. ) ;
#4173 = EDGE_CURVE ( 'NONE', #2638, #5335, #3623, .T. ) ;
#4174 = SURFACE_STYLE_FILL_AREA ( #6739 ) ;
#4175 = CARTESIAN_POINT ( 'NONE',  ( 352.0000000000000000, -20.00000000000000000, -16.23142504031546807 ) ) ;
#4176 = ORIENTED_EDGE ( 'NONE', *, *, #6462, .F. ) ;
#4177 = VERTEX_POINT ( 'NONE', #2289 ) ;
#4178 = CARTESIAN_POINT ( 'NONE',  ( -4.236525694536558362, 2.416953475386465211, -3.751298745799836354 ) ) ;
#4179 = LINE ( 'NONE', #6831, #7574 ) ;
#4180 = DIRECTION ( 'NONE',  ( -1.000000000000000000, 0.000000000000000000, -0.000000000000000000 ) ) ;
#4181 = LINE ( 'NONE', #4229, #2764 ) ;
#4182 = ORIENTED_EDGE ( 'NONE', *, *, #1919, .F. ) ;
#4183 = CARTESIAN_POINT ( 'NONE',  ( -2.805705207896067144, 3.226868319750155312, -3.503898532754364581 ) ) ;
#4184 = DIRECTION ( 'NONE',  ( 1.000000000000000000, 0.000000000000000000, 0.000000000000000000 ) ) ;
#4185 = CARTESIAN_POINT ( 'NONE',  ( 0.000000000000000000, 0.000000000000000000, 62.00000000000001421 ) ) ;
#4186 = APPLICATION_CONTEXT ( 'automotive_design' ) ;
#4187 = CARTESIAN_POINT ( 'NONE',  ( 5.000000000000000000, -5.000000000000000000, -97.99999999999997158 ) ) ;
#4188 = FACE_OUTER_BOUND ( 'NONE', #4988, .T. ) ;
#4189 = CARTESIAN_POINT ( 'NONE',  ( 2.500000000000000000, -2.629050547790028551E-15, -2.041999999999999815 ) ) ;
#4190 = PRODUCT_DEFINITION_FORMATION_WITH_SPECIFIED_SOURCE ( 'ANY', '', #6621, .NOT_KNOWN. ) ;
#4191 = VERTEX_POINT ( 'NONE', #3068 ) ;
#4192 = ORIENTED_EDGE ( 'NONE', *, *, #6939, .T. ) ;
#4193 = EDGE_CURVE ( 'NONE', #6781, #5745, #5752, .T. ) ;
#4194 = ADVANCED_FACE ( 'NONE', ( #1805 ), #3848, .F. ) ;
#4195 = EDGE_LOOP ( 'NONE', ( #862, #4405 ) ) ;
#4196 = DIRECTION ( 'NONE',  ( 1.000000000000000000, 1.734723475976806848E-16, 0.000000000000000000 ) ) ;
#4197 = ADVANCED_FACE ( 'NONE', ( #7850 ), #3152, .T. ) ;
#4198 = CARTESIAN_POINT ( 'NONE',  ( 2.500000000000000000, -1.178949249685218303, -2.041999999999998039 ) ) ;
#4199 = CIRCLE ( 'NONE', #6560, 10.00000000000000000 ) ;
#4200 = EDGE_LOOP ( 'NONE', ( #6003, #7461, #1222, #8323, #6112 ) ) ;
#4201 = DIRECTION ( 'NONE',  ( -1.000000000000000000, 0.000000000000000000, -0.000000000000000000 ) ) ;
#4202 = CIRCLE ( 'NONE', #453, 2.649999999999985700 ) ;
#4203 = ORIENTED_EDGE ( 'NONE', *, *, #7177, .T. ) ;
#4204 = DIRECTION ( 'NONE',  ( 1.000000000000000000, 0.000000000000000000, 0.000000000000000000 ) ) ;
#4205 = CIRCLE ( 'NONE', #3658, 2.649999999999985700 ) ;
#4206 = DIRECTION ( 'NONE',  ( 0.000000000000000000, -0.000000000000000000, 1.000000000000000000 ) ) ;
#4207 = APPLICATION_PROTOCOL_DEFINITION ( 'draft international standard', 'automotive_design', 1998, #2860 ) ;
#4208 = FILL_AREA_STYLE ('',( #777 ) ) ;
#4209 = VERTEX_POINT ( 'NONE', #4492 ) ;
#4210 = VECTOR ( 'NONE', #2662, 1000.000000000000000 ) ;
#4211 = EDGE_LOOP ( 'NONE', ( #7619, #5605, #4671, #2540 ) ) ;
#4212 = DIRECTION ( 'NONE',  ( -0.000000000000000000, -0.000000000000000000, -1.000000000000000000 ) ) ;
#4213 = EDGE_CURVE ( 'NONE', #8098, #7561, #3108, .T. ) ;
#4214 = COLOUR_RGB ( '',1.000000000000000000, 0.9490196078431372140, 0.9098039215686274384 ) ;
#4215 = CARTESIAN_POINT ( 'NONE',  ( -0.6666666666666651864, 4.233901974057260098, -3.300726591567081147 ) ) ;
#4216 = AXIS2_PLACEMENT_3D ( 'NONE', #1294, #4474, #7131 ) ;
#4217 = CARTESIAN_POINT ( 'NONE',  ( 347.0000000000000000, -4.999999999999998224, 140.0000000000000000 ) ) ;
#4218 = CARTESIAN_POINT ( 'NONE',  ( 181.0000000000000000, -4.999999999999998224, 140.0000000000000000 ) ) ;
#4219 = ORIENTED_EDGE ( 'NONE', *, *, #1751, .T. ) ;
#4220 = AXIS2_PLACEMENT_3D ( 'NONE', #4387, #7124, #6387 ) ;
#4221 =( NAMED_UNIT ( * ) SI_UNIT ( $, .STERADIAN. ) SOLID_ANGLE_UNIT ( ) );
#4222 = CARTESIAN_POINT ( 'NONE',  ( 0.000000000000000000, 0.000000000000000000, 0.000000000000000000 ) ) ;
#4223 = ORIENTED_EDGE ( 'NONE', *, *, #668, .T. ) ;
#4224 = DIRECTION ( 'NONE',  ( 0.000000000000000000, 0.000000000000000000, 1.000000000000000000 ) ) ;
#4225 = CARTESIAN_POINT ( 'NONE',  ( 10.00000000000000000, 0.000000000000000000, -27.99999999999999645 ) ) ;
#4226 = EDGE_CURVE ( 'NONE', #4209, #4673, #2919, .T. ) ;
#4227 = VECTOR ( 'NONE', #7735, 1000.000000000000000 ) ;
#4228 = DIRECTION ( 'NONE',  ( 0.8191520442889902442, 1.003171929053522651E-16, -0.5735764363510482688 ) ) ;
#4229 = CARTESIAN_POINT ( 'NONE',  ( 3.245314017740478073E-16, -20.00000000000000000, -160.1500000000000057 ) ) ;
#4230 = ORIENTED_EDGE ( 'NONE', *, *, #1244, .T. ) ;
#4231 = CARTESIAN_POINT ( 'NONE',  ( -5.000000000000001776, 5.000000000000001776, 148.0000000000000284 ) ) ;
#4232 =( NAMED_UNIT ( * ) PLANE_ANGLE_UNIT ( ) SI_UNIT ( $, .RADIAN. ) );
#4233 = CIRCLE ( 'NONE', #188, 2.041999999999999815 ) ;
#4234 = DIRECTION ( 'NONE',  ( 0.000000000000000000, 1.000000000000000000, 0.000000000000000000 ) ) ;
#4235 = ADVANCED_FACE ( 'NONE', ( #8468 ), #5146, .T. ) ;
#4236 = LINE ( 'NONE', #7726, #2951 ) ;
#4237 = CARTESIAN_POINT ( 'NONE',  ( -31.74999999999995737, 0.000000000000000000, 0.000000000000000000 ) ) ;
#4238 = CARTESIAN_POINT ( 'NONE',  ( -2.756197834950067094, -3.027510591568735254, -3.223146290109809797 ) ) ;
#4239 = DIRECTION ( 'NONE',  ( -1.734723475976807341E-16, 1.000000000000000000, 0.000000000000000000 ) ) ;
#4240 = ORIENTED_EDGE ( 'NONE', *, *, #3038, .F. ) ;
#4241 = ORIENTED_EDGE ( 'NONE', *, *, #706, .T. ) ;
#4242 = ORIENTED_EDGE ( 'NONE', *, *, #1504, .T. ) ;
#4243 = CARTESIAN_POINT ( 'NONE',  ( -20.00000000000000000, 140.0000000000000000, 5.000000000000000000 ) ) ;
#4244 = FILL_AREA_STYLE_COLOUR ( '', #5050 ) ;
#4245 = EDGE_CURVE ( 'NONE', #8587, #8492, #7728, .T. ) ;
#4246 = EDGE_CURVE ( 'NONE', #2638, #3461, #7060, .T. ) ;
#4247 = ORIENTED_EDGE ( 'NONE', *, *, #6939, .F. ) ;
#4248 = CIRCLE ( 'NONE', #6745, 20.00000000000000000 ) ;
#4249 = VERTEX_POINT ( 'NONE', #1145 ) ;
#4250 =( NAMED_UNIT ( * ) PLANE_ANGLE_UNIT ( ) SI_UNIT ( $, .RADIAN. ) );
#4251 = CARTESIAN_POINT ( 'NONE',  ( 439.9999999999999432, -20.00000000000000000, 18.96857495968446017 ) ) ;
#4252 = PRODUCT_CONTEXT ( 'NONE', #6415, 'mechanical' ) ;
#4253 = ORIENTED_EDGE ( 'NONE', *, *, #5665, .T. ) ;
#4254 = EDGE_LOOP ( 'NONE', ( #4856, #5154, #8478, #3929 ) ) ;
#4255 = LINE ( 'NONE', #2866, #6141 ) ;
#4256 = CYLINDRICAL_SURFACE ( 'NONE', #6153, 2.649999999999985700 ) ;
#4257 = AXIS2_PLACEMENT_3D ( 'NONE', #1508, #8265, #4156 ) ;
#4258 = VECTOR ( 'NONE', #7958, 1000.000000000000000 ) ;
#4259 = CARTESIAN_POINT ( 'NONE',  ( -1.391697335622809950, -4.043246145443391448, -3.503898532754372575 ) ) ;
#4260 = DIRECTION ( 'NONE',  ( -0.000000000000000000, -0.000000000000000000, 1.000000000000000000 ) ) ;
#4261 = EDGE_CURVE ( 'NONE', #3640, #1009, #1113, .T. ) ;
#4262 = ORIENTED_EDGE ( 'NONE', *, *, #6635, .T. ) ;
#4263 = AXIS2_PLACEMENT_3D ( 'NONE', #3205, #5275, #7944 ) ;
#4264 = AXIS2_PLACEMENT_3D ( 'NONE', #417, #6465, #8479 ) ;
#4265 = CARTESIAN_POINT ( 'NONE',  ( -4.999999999999999112, 140.0000000000000000, 25.00000000000000000 ) ) ;
#4266 = ORIENTED_EDGE ( 'NONE', *, *, #7307, .F. ) ;
#4267 = CARTESIAN_POINT ( 'NONE',  ( -1.257172072275743346, 3.892973519171203378, -3.433252694550776862 ) ) ;
#4268 = FACE_BOUND ( 'NONE', #4796, .T. ) ;
#4269 = TOROIDAL_SURFACE ( 'NONE', #5513, 5.384454397937118664, 0.5155456020628804703 ) ;
#4270 = VECTOR ( 'NONE', #6735, 1000.000000000000000 ) ;
#4271 = CARTESIAN_POINT ( 'NONE',  ( 434.9999999999999432, 5.000000000000001776, 140.0000000000000000 ) ) ;
#4272 = DIRECTION ( 'NONE',  ( 0.000000000000000000, 0.000000000000000000, 1.000000000000000000 ) ) ;
#4273 = ORIENTED_EDGE ( 'NONE', *, *, #3295, .F. ) ;
#4274 = PLANE ( 'NONE',  #1808 ) ;
#4275 = PRODUCT_DEFINITION_SHAPE ( 'NONE', 'NONE',  #8630 ) ;
#4276 = DIRECTION ( 'NONE',  ( 1.000000000000000000, 0.000000000000000000, 0.000000000000000000 ) ) ;
#4277 = CARTESIAN_POINT ( 'NONE',  ( 439.9999999999999432, -20.00000000000000000, 18.96857495968446017 ) ) ;
#4278 = EDGE_CURVE ( 'NONE', #6761, #6694, #403, .T. ) ;
#4279 = LINE ( 'NONE', #1585, #840 ) ;
#4280 = EDGE_CURVE ( 'NONE', #2382, #8131, #7083, .T. ) ;
#4281 = CARTESIAN_POINT ( 'NONE',  ( 0.000000000000000000, 0.000000000000000000, 120.0000000000000000 ) ) ;
#4282 = CARTESIAN_POINT ( 'NONE',  ( -4.000000000000000000, -0.8232339106130515116, -3.430630286862743183 ) ) ;
#4283 = EDGE_LOOP ( 'NONE', ( #1305, #5498, #2681, #6760 ) ) ;
#4284 = EDGE_CURVE ( 'NONE', #6072, #2349, #8208, .T. ) ;
#4285 = ORIENTED_EDGE ( 'NONE', *, *, #1348, .F. ) ;
#4286 = ORIENTED_EDGE ( 'NONE', *, *, #5570, .T. ) ;
#4287 = PLANE ( 'NONE',  #7842 ) ;
#4288 = LINE ( 'NONE', #5110, #749 ) ;
#4289 = AXIS2_PLACEMENT_3D ( 'NONE', #1183, #1667, #1097 ) ;
#4290 = EDGE_LOOP ( 'NONE', ( #4385, #646, #4422, #3883 ) ) ;
#4291 = CARTESIAN_POINT ( 'NONE',  ( 5.000000000000000000, 5.000000000000000000, -27.99999999999999645 ) ) ;
#4292 = EDGE_LOOP ( 'NONE', ( #4157, #4893, #7142, #3385 ) ) ;
#4293 =( LENGTH_UNIT ( ) NAMED_UNIT ( * ) SI_UNIT ( .MILLI., .METRE. ) );
#4294 = DIRECTION ( 'NONE',  ( 0.000000000000000000, -1.000000000000000000, 0.000000000000000000 ) ) ;
#4295 = ITEM_DEFINED_TRANSFORMATION ( 'NONE', 'NONE', #6972,  #594 ) ;
#4296 = ORIENTED_EDGE ( 'NONE', *, *, #6919, .F. ) ;
#4297 = EDGE_LOOP ( 'NONE', ( #7599, #4151, #3947, #1204 ) ) ;
#4298 = EDGE_CURVE ( 'NONE', #7568, #5774, #8381, .T. ) ;
#4299 = CARTESIAN_POINT ( 'NONE',  ( -4.211140560182196957, 2.431303136016537803, -3.745885042887433514 ) ) ;
#4300 = CIRCLE ( 'NONE', #539, 2.649999999999985700 ) ;
#4301 = FACE_OUTER_BOUND ( 'NONE', #4124, .T. ) ;
#4302 = CARTESIAN_POINT ( 'NONE',  ( 53.33333333333330017, -20.00000000000000000, 162.5000000000000853 ) ) ;
#4303 = CIRCLE ( 'NONE', #971, 20.00000000000000000 ) ;
#4304 = CARTESIAN_POINT ( 'NONE',  ( 5.384454397937118664, 0.000000000000000000, -4.484454397937119197 ) ) ;
#4305 = ORIENTED_EDGE ( 'NONE', *, *, #3989, .T. ) ;
#4306 = CARTESIAN_POINT ( 'NONE',  ( 439.9999999999999432, 0.000000000000000000, 0.000000000000000000 ) ) ;
#4307 = DIRECTION ( 'NONE',  ( -1.734723475976807587E-16, 1.000000000000000000, 0.000000000000000000 ) ) ;
#4308 = ORIENTED_EDGE ( 'NONE', *, *, #2485, .F. ) ;
#4309 = EDGE_LOOP ( 'NONE', ( #6401, #7789, #4734, #4963 ) ) ;
#4310 = DIRECTION ( 'NONE',  ( -1.000000000000000000, 0.000000000000000000, 0.000000000000000000 ) ) ;
#4311 = ADVANCED_FACE ( 'NONE', ( #533 ), #1761, .T. ) ;
#4312 = CARTESIAN_POINT ( 'NONE',  ( 93.00000000000000000, -4.999999999999998224, 139.9990000000000236 ) ) ;
#4313 = EDGE_CURVE ( 'NONE', #8098, #2697, #2424, .T. ) ;
#4314 = LINE ( 'NONE', #1531, #1911 ) ;
#4315 = CARTESIAN_POINT ( 'NONE',  ( 5.000000000000000000, -5.000000000000000000, 34.00000000000000711 ) ) ;
#4316 = EDGE_LOOP ( 'NONE', ( #7225, #521, #7494, #3289 ) ) ;
#4317 = DIRECTION ( 'NONE',  ( 0.000000000000000000, 1.000000000000000000, 0.000000000000000000 ) ) ;
#4318 =( LENGTH_UNIT ( ) NAMED_UNIT ( * ) SI_UNIT ( .MILLI., .METRE. ) );
#4319 = VERTEX_POINT ( 'NONE', #1060 ) ;
#4320 = CYLINDRICAL_SURFACE ( 'NONE', #6143, 2.649999999999985700 ) ;
#4321 = DIRECTION ( 'NONE',  ( -1.734723475976806848E-16, 1.000000000000000000, 0.000000000000000000 ) ) ;
#4322 = CARTESIAN_POINT ( 'NONE',  ( -10.00000000000000000, 1.224646799147353256E-15, -135.0000000000000000 ) ) ;
#4323 = DIRECTION ( 'NONE',  ( -1.000000000000000000, 0.000000000000000000, 0.000000000000000000 ) ) ;
#4324 = CARTESIAN_POINT ( 'NONE',  ( -4.197477534772231955, 0.8522413273724368521, -3.505042416683225692 ) ) ;
#4325 = ORIENTED_EDGE ( 'NONE', *, *, #2847, .T. ) ;
#4326 = ORIENTED_EDGE ( 'NONE', *, *, #445, .F. ) ;
#4327 = PRESENTATION_LAYER_ASSIGNMENT (  '', '', ( #7674 ) ) ;
#4328 = ORIENTED_EDGE ( 'NONE', *, *, #1751, .F. ) ;
#4329 = PLANE ( 'NONE',  #8538 ) ;
#4330 = EDGE_CURVE ( 'NONE', #2249, #3505, #3715, .T. ) ;
#4331 = DIRECTION ( 'NONE',  ( -0.000000000000000000, -0.000000000000000000, 1.000000000000000000 ) ) ;
#4332 = ADVANCED_FACE ( 'NONE', ( #444 ), #5014, .T. ) ;
#4333 = DIRECTION ( 'NONE',  ( -5.913326431989248494E-18, -0.9999999999999998890, -2.774927572856598806E-16 ) ) ;
#4334 = ORIENTED_EDGE ( 'NONE', *, *, #2002, .F. ) ;
#4335 = CARTESIAN_POINT ( 'NONE',  ( 303.3333333333333144, -20.00000000000000000, 162.5000000000000853 ) ) ;
#4336 = ORIENTED_EDGE ( 'NONE', *, *, #4872, .T. ) ;
#4337 = LINE ( 'NONE', #2252, #649 ) ;
#4338 = ORIENTED_EDGE ( 'NONE', *, *, #3159, .F. ) ;
#4339 = VERTEX_POINT ( 'NONE', #6956 ) ;
#4340 = DIRECTION ( 'NONE',  ( 0.000000000000000000, 0.000000000000000000, 1.000000000000000000 ) ) ;
#4341 = LINE ( 'NONE', #3646, #3244 ) ;
#4342 = VECTOR ( 'NONE', #4022, 1000.000000000000000 ) ;
#4343 = DIRECTION ( 'NONE',  ( 0.000000000000000000, 0.000000000000000000, -1.000000000000000000 ) ) ;
#4344 = DIRECTION ( 'NONE',  ( 0.000000000000000000, 0.000000000000000000, -1.000000000000000000 ) ) ;
#4345 = ORIENTED_EDGE ( 'NONE', *, *, #830, .T. ) ;
#4346 = AXIS2_PLACEMENT_3D ( 'NONE', #5532, #6794, #8205 ) ;
#4347 = DIRECTION ( 'NONE',  ( 1.000000000000000000, 0.000000000000000000, 0.000000000000000000 ) ) ;
#4348 = FACE_OUTER_BOUND ( 'NONE', #2492, .T. ) ;
#4349 = EDGE_LOOP ( 'NONE', ( #1725, #6374 ) ) ;
#4350 = VERTEX_POINT ( 'NONE', #5693 ) ;
#4351 = AXIS2_PLACEMENT_3D ( 'NONE', #1510, #5380, #4204 ) ;
#4352 = DIRECTION ( 'NONE',  ( 0.000000000000000000, 0.000000000000000000, -1.000000000000000000 ) ) ;
#4353 = DIRECTION ( 'NONE',  ( -0.000000000000000000, -0.000000000000000000, 1.000000000000000000 ) ) ;
#4354 = VECTOR ( 'NONE', #2495, 1000.000000000000114 ) ;
#4355 = VECTOR ( 'NONE', #2601, 1000.000000000000000 ) ;
#4356 = DIRECTION ( 'NONE',  ( -1.000000000000000000, 0.000000000000000000, 0.000000000000000000 ) ) ;
#4357 = ADVANCED_FACE ( 'NONE', ( #3051 ), #5651, .F. ) ;
#4358 = CARTESIAN_POINT ( 'NONE',  ( 170.9999999999999716, 5.000000000000001776, 140.0000000000000000 ) ) ;
#4359 = ORIENTED_EDGE ( 'NONE', *, *, #2409, .T. ) ;
#4360 = EDGE_CURVE ( 'NONE', #5286, #6478, #7792, .T. ) ;
#4361 = DIRECTION ( 'NONE',  ( 0.000000000000000000, 0.000000000000000000, 1.000000000000000000 ) ) ;
#4362 = APPLICATION_PROTOCOL_DEFINITION ( 'draft international standard', 'automotive_design', 1998, #3917 ) ;
#4363 = ORIENTED_EDGE ( 'NONE', *, *, #7820, .T. ) ;
#4364 =( REPRESENTATION_RELATIONSHIP ('NONE','NONE', #3312, #872 ) REPRESENTATION_RELATIONSHIP_WITH_TRANSFORMATION ( #4295 )SHAPE_REPRESENTATION_RELATIONSHIP( ) );
#4365 = CARTESIAN_POINT ( 'NONE',  ( -4.999999999999998224, -4.999999999999998224, 139.9990000000000236 ) ) ;
#4366 = VECTOR ( 'NONE', #6498, 1000.000000000000000 ) ;
#4367 = CARTESIAN_POINT ( 'NONE',  ( 20.00000000000000000, 0.000000000000000000, 120.0000000000000142 ) ) ;
#4368 = CARTESIAN_POINT ( 'NONE',  ( -20.00000000000000000, 135.0000000000000000, 40.00000000000000000 ) ) ;
#4369 = CARTESIAN_POINT ( 'NONE',  ( 170.9999999999999716, -4.999999999999998224, 140.0000000000000000 ) ) ;
#4370 = CARTESIAN_POINT ( 'NONE',  ( 259.0000000000000000, -4.999999999999998224, 139.9990000000000236 ) ) ;
#4371 = VECTOR ( 'NONE', #1299, 1000.000000000000000 ) ;
#4373 = ORIENTED_EDGE ( 'NONE', *, *, #8506, .F. ) ;
#4372 = EDGE_CURVE ( 'NONE', #8282, #2200, #4036, .T. ) ;
#4374 = ORIENTED_EDGE ( 'NONE', *, *, #6559, .T. ) ;
#4375 = DIRECTION ( 'NONE',  ( 1.000000000000000000, 0.000000000000000000, 1.734723475976807587E-16 ) ) ;
#4376 = DIRECTION ( 'NONE',  ( -0.000000000000000000, -0.000000000000000000, 1.000000000000000000 ) ) ;
#4377 = UNCERTAINTY_MEASURE_WITH_UNIT (LENGTH_MEASURE( 1.000000000000000082E-05 ), #115, 'distance_accuracy_value', 'NONE');
#4378 = CIRCLE ( 'NONE', #1596, 2.700000000000001066 ) ;
#4379 = VERTEX_POINT ( 'NONE', #5732 ) ;
#4380 = CARTESIAN_POINT ( 'NONE',  ( -5.000000000000000000, -5.000000000000000000, 148.0000000000000284 ) ) ;
#4381 = ORIENTED_EDGE ( 'NONE', *, *, #7415, .F. ) ;
#4382 = FILL_AREA_STYLE_COLOUR ( '', #3662 ) ;
#4383 = DIRECTION ( 'NONE',  ( -0.9284766908852593037, 0.000000000000000000, -0.3713906763541036660 ) ) ;
#4384 = EDGE_LOOP ( 'NONE', ( #395, #6384 ) ) ;
#4385 = ORIENTED_EDGE ( 'NONE', *, *, #7333, .T. ) ;
#4386 = PLANE ( 'NONE',  #1191 ) ;
#4387 = CARTESIAN_POINT ( 'NONE',  ( 0.000000000000000000, 0.000000000000000000, -4.974599999999998801 ) ) ;
#4388 = ADVANCED_FACE ( 'NONE', ( #2491, #5129 ), #3089, .T. ) ;
#4389 = CARTESIAN_POINT ( 'NONE',  ( 4.000000000000000000, 2.309401076758497151, -3.433295621305379353 ) ) ;
#4390 = CARTESIAN_POINT ( 'NONE',  ( 5.000000000000001776, 135.0000000000000000, 15.00000000000000355 ) ) ;
#4391 = EDGE_CURVE ( 'NONE', #563, #6628, #3340, .T. ) ;
#4392 = VERTEX_POINT ( 'NONE', #8280 ) ;
#4393 = DIRECTION ( 'NONE',  ( 0.000000000000000000, 0.000000000000000000, 1.000000000000000000 ) ) ;
#4394 = FACE_BOUND ( 'NONE', #2147, .T. ) ;
#4395 = ORIENTED_EDGE ( 'NONE', *, *, #5520, .T. ) ;
#4396 = EDGE_CURVE ( 'NONE', #4853, #5335, #2958, .T. ) ;
#4397 = ORIENTED_EDGE ( 'NONE', *, *, #6376, .T. ) ;
#4398 = CIRCLE ( 'NONE', #1328, 2.500000000000001332 ) ;
#4399 = DIRECTION ( 'NONE',  ( -0.000000000000000000, -0.000000000000000000, -1.000000000000000000 ) ) ;
#4400 = CARTESIAN_POINT ( 'NONE',  ( -5.000000000000001776, 5.000000000000001776, -63.99999999999997158 ) ) ;
#4401 = CARTESIAN_POINT ( 'NONE',  ( 10.00000000000000000, 0.000000000000000000, -135.0000000000000000 ) ) ;
#4402 = VECTOR ( 'NONE', #6333, 1000.000000000000000 ) ;
#4403 = CARTESIAN_POINT ( 'NONE',  ( 0.000000000000000000, 0.000000000000000000, 42.00000000000000711 ) ) ;
#4404 = ORIENTED_EDGE ( 'NONE', *, *, #4360, .T. ) ;
#4405 = ORIENTED_EDGE ( 'NONE', *, *, #1539, .F. ) ;
#4406 = DIRECTION ( 'NONE',  ( 0.000000000000000000, 0.000000000000000000, -1.000000000000000000 ) ) ;
#4407 = PRESENTATION_LAYER_ASSIGNMENT (  '', '', ( #8164 ) ) ;
#4408 = ADVANCED_FACE ( 'NONE', ( #4348 ), #4434, .T. ) ;
#4409 = AXIS2_PLACEMENT_3D ( 'NONE', #5007, #4180, #258 ) ;
#4410 = CARTESIAN_POINT ( 'NONE',  ( 259.0000000000000000, 5.000000000000001776, 145.0000000000000284 ) ) ;
#4411 = DIRECTION ( 'NONE',  ( 0.000000000000000000, -0.000000000000000000, 1.000000000000000000 ) ) ;
#4412 = CARTESIAN_POINT ( 'NONE',  ( 5.000000000000000000, 5.000000000000000000, 140.0000000000000000 ) ) ;
#4413 = CARTESIAN_POINT ( 'NONE',  ( -4.000000000000000000, 2.511478553582031203, -3.469254451724764543 ) ) ;
#4414 = EDGE_LOOP ( 'NONE', ( #7777, #7162 ) ) ;
#4415 = DIRECTION ( 'NONE',  ( 1.000000000000000000, 0.000000000000000000, 0.000000000000000000 ) ) ;
#4416 = FACE_OUTER_BOUND ( 'NONE', #791, .T. ) ;
#4417 = FACE_OUTER_BOUND ( 'NONE', #1446, .T. ) ;
#4418 = DIRECTION ( 'NONE',  ( -0.000000000000000000, -0.000000000000000000, 1.000000000000000000 ) ) ;
#4419 = PRODUCT_DEFINITION_SHAPE ( 'NONE', 'NONE',  #8624 ) ;
#4420 = EDGE_LOOP ( 'NONE', ( #2853, #8009, #4877, #3773 ) ) ;
#4421 = LINE ( 'NONE', #4291, #3704 ) ;
#4422 = ORIENTED_EDGE ( 'NONE', *, *, #1810, .F. ) ;
#4423 = CARTESIAN_POINT ( 'NONE',  ( 0.000000000000000000, 0.000000000000000000, 7.000000000000006217 ) ) ;
#4424 = ORIENTED_EDGE ( 'NONE', *, *, #6500, .T. ) ;
#4425 = ORIENTED_EDGE ( 'NONE', *, *, #668, .F. ) ;
#4426 = CARTESIAN_POINT ( 'NONE',  ( -4.197393957002303999, 0.4069871074557429025, -3.503767560748926257 ) ) ;
#4427 = DIRECTION ( 'NONE',  ( 1.734723475976806848E-16, -1.000000000000000000, -0.000000000000000000 ) ) ;
#4428 = VECTOR ( 'NONE', #2328, 1000.000000000000000 ) ;
#4429 = FACE_OUTER_BOUND ( 'NONE', #425, .T. ) ;
#4430 = VERTEX_POINT ( 'NONE', #477 ) ;
#4431 = ADVANCED_FACE ( 'NONE', ( #5000 ), #6345, .F. ) ;
#4432 = CIRCLE ( 'NONE', #399, 4.000000000000000000 ) ;
#4433 = CARTESIAN_POINT ( 'NONE',  ( 386.6666666666666288, -10.00000000000000000, 162.5000000000000853 ) ) ;
#4434 = CYLINDRICAL_SURFACE ( 'NONE', #274, 10.00000000000000000 ) ;
#4435 = ORIENTED_EDGE ( 'NONE', *, *, #5862, .F. ) ;
#4436 = ORIENTED_EDGE ( 'NONE', *, *, #8204, .F. ) ;
#4437 = ADVANCED_FACE ( 'NONE', ( #8411 ), #7665, .F. ) ;
#4438 = CARTESIAN_POINT ( 'NONE',  ( 386.6666666666666288, -20.00000000000000000, 159.8500000000001080 ) ) ;
#4439 = DIRECTION ( 'NONE',  ( 1.000000000000000000, 0.000000000000000000, 0.000000000000000000 ) ) ;
#4440 = ADVANCED_FACE ( 'NONE', ( #1792 ), #5043, .T. ) ;
#4441 = AXIS2_PLACEMENT_3D ( 'NONE', #3620, #2148, #3537 ) ;
#4442 = ADVANCED_FACE ( 'NONE', ( #6914, #4394 ), #340, .F. ) ;
#4443 = FACE_OUTER_BOUND ( 'NONE', #2890, .T. ) ;
#4444 = DIRECTION ( 'NONE',  ( -0.8660254037844377084, -0.5000000000000015543, 0.000000000000000000 ) ) ;
#4445 = ORIENTED_EDGE ( 'NONE', *, *, #5706, .F. ) ;
#4446 = VERTEX_POINT ( 'NONE', #961 ) ;
#4447 = AXIS2_PLACEMENT_3D ( 'NONE', #7150, #5795, #1190 ) ;
#4448 = LINE ( 'NONE', #490, #7695 ) ;
#4449 = DIRECTION ( 'NONE',  ( 1.000000000000000000, -1.734723475976806848E-16, 0.000000000000000000 ) ) ;
#4450 = AXIS2_PLACEMENT_3D ( 'NONE', #7754, #1087, #3698 ) ;
#4451 = DIRECTION ( 'NONE',  ( 0.000000000000000000, -0.000000000000000000, 1.000000000000000000 ) ) ;
#4452 = DIRECTION ( 'NONE',  ( 0.000000000000000000, 0.000000000000000000, 1.000000000000000000 ) ) ;
#4453 = LINE ( 'NONE', #5577, #2602 ) ;
#4454 = ORIENTED_EDGE ( 'NONE', *, *, #5495, .T. ) ;
#4455 = SURFACE_STYLE_USAGE ( .BOTH. , #3114 ) ;
#4456 = DIRECTION ( 'NONE',  ( -1.000000000000000000, 0.000000000000000000, -0.000000000000000000 ) ) ;
#4457 = CARTESIAN_POINT ( 'NONE',  ( 219.9999999999999716, -20.00000000000000000, 162.5000000000000853 ) ) ;
#4458 = DIRECTION ( 'NONE',  ( -0.000000000000000000, -0.000000000000000000, 1.000000000000000000 ) ) ;
#4459 = ADVANCED_FACE ( 'NONE', ( #7002 ), #6260, .F. ) ;
#4460 = ORIENTED_EDGE ( 'NONE', *, *, #6210, .F. ) ;
#4461 = EDGE_CURVE ( 'NONE', #8171, #5488, #2360, .T. ) ;
#4462 = CARTESIAN_POINT ( 'NONE',  ( -5.000000000000000000, -5.000000000000000000, 148.0000000000000284 ) ) ;
#4463 = ITEM_DEFINED_TRANSFORMATION ( 'NONE', 'NONE', #2669,  #594 ) ;
#4464 = EDGE_LOOP ( 'NONE', ( #8258, #68, #1789, #2767 ) ) ;
#4465 = EDGE_CURVE ( 'NONE', #6101, #1747, #1996, .T. ) ;
#4466 = ORIENTED_EDGE ( 'NONE', *, *, #2128, .F. ) ;
#4467 = CARTESIAN_POINT ( 'NONE',  ( 4.000000000000000000, 2.309401076758515803, -0.4999999999999995559 ) ) ;
#4468 = CARTESIAN_POINT ( 'NONE',  ( -5.000000000000000000, -5.000000000000000000, 148.0000000000000284 ) ) ;
#4469 = CARTESIAN_POINT ( 'NONE',  ( -5.000000000000000000, -5.000000000000000000, -0.9999999999999940048 ) ) ;
#4470 = ORIENTED_EDGE ( 'NONE', *, *, #1539, .T. ) ;
#4471 = AXIS2_PLACEMENT_3D ( 'NONE', #3651, #4472, #1745 ) ;
#4472 = DIRECTION ( 'NONE',  ( 0.000000000000000000, 0.000000000000000000, 1.000000000000000000 ) ) ;
#4473 = EDGE_CURVE ( 'NONE', #3882, #5424, #21, .T. ) ;
#4474 = DIRECTION ( 'NONE',  ( 0.000000000000000000, 0.000000000000000000, -1.000000000000000000 ) ) ;
#4475 = ORIENTED_EDGE ( 'NONE', *, *, #1653, .T. ) ;
#4476 = ORIENTED_EDGE ( 'NONE', *, *, #5828, .F. ) ;
#4477 = PLANE ( 'NONE',  #7703 ) ;
#4478 =( BOUNDED_SURFACE ( )  B_SPLINE_SURFACE ( 3, 2, ( 
 ( #3967, #2704, #1963 ),
 ( #4093, #3918, #5346 ),
 ( #1256, #6562, #5296 ),
 ( #4602, #5947, #2655 ),
 ( #2053, #7970, #8060 ),
 ( #2010, #4649, #7308 ) ),
 .UNSPECIFIED., .F., .F., .F. ) 
 B_SPLINE_SURFACE_WITH_KNOTS ( ( 4, 2, 4 ),
 ( 3, 3 ),
 ( 0.02027065861071770947, 0.02273072267836921331, 0.02519078674602071716 ),
 ( 0.000000000000000000, 1.000000000000000000 ),
 .UNSPECIFIED. ) 
 GEOMETRIC_REPRESENTATION_ITEM ( )  RATIONAL_B_SPLINE_SURFACE ( (
 ( 1.000000000000000000, 0.8047781708337304885, 1.000000000000000000),
 ( 1.000000000000000000, 0.8123765190705307671, 1.000000000000000000),
 ( 1.000000000000000000, 0.8190656277163975707, 1.000000000000000000),
 ( 1.000000000000000000, 0.8192366903512159348, 1.000000000000000000),
 ( 1.000000000000000000, 0.8126138454302893610, 1.000000000000000000),
 ( 1.000000000000000000, 0.8047712246031417660, 1.000000000000000000) ) ) 
 REPRESENTATION_ITEM ( '' )  SURFACE ( )  );
#4479 = DIRECTION ( 'NONE',  ( 0.000000000000000000, 0.000000000000000000, 1.000000000000000000 ) ) ;
#4480 = VECTOR ( 'NONE', #3498, 1000.000000000000000 ) ;
#4481 = VECTOR ( 'NONE', #7498, 1000.000000000000000 ) ;
#4482 = DIRECTION ( 'NONE',  ( 0.000000000000000000, 0.000000000000000000, -1.000000000000000000 ) ) ;
#4483 = DIRECTION ( 'NONE',  ( 1.000000000000000000, 1.734723475976806848E-16, 0.000000000000000000 ) ) ;
#4484 = ORIENTED_EDGE ( 'NONE', *, *, #7478, .F. ) ;
#4485 = ORIENTED_EDGE ( 'NONE', *, *, #4994, .T. ) ;
#4486 = ORIENTED_EDGE ( 'NONE', *, *, #1593, .F. ) ;
#4487 = FACE_OUTER_BOUND ( 'NONE', #1312, .T. ) ;
#4488 = CIRCLE ( 'NONE', #6295, 2.649999999999985700 ) ;
#4489 = EDGE_CURVE ( 'NONE', #6097, #8421, #2000, .T. ) ;
#4490 = VECTOR ( 'NONE', #547, 1000.000000000000000 ) ;
#4491 = FACE_BOUND ( 'NONE', #3726, .T. ) ;
#4492 = CARTESIAN_POINT ( 'NONE',  ( 2.500000000000000444, 0.000000000000000000, -5.000000000000000888 ) ) ;
#4493 = DIRECTION ( 'NONE',  ( -0.000000000000000000, -0.000000000000000000, -1.000000000000000000 ) ) ;
#4494 = DIRECTION ( 'NONE',  ( -0.000000000000000000, 1.000000000000000000, -0.000000000000000000 ) ) ;
#4495 = EDGE_CURVE ( 'NONE', #8491, #437, #7976, .T. ) ;
#4496 = AXIS2_PLACEMENT_3D ( 'NONE', #3683, #5676, #2387 ) ;
#4497 = COLOUR_RGB ( '',1.000000000000000000, 0.9490196078431372140, 0.9098039215686274384 ) ;
#4498 = DIRECTION ( 'NONE',  ( -0.000000000000000000, 1.000000000000000000, -0.000000000000000000 ) ) ;
#4499 = EDGE_CURVE ( 'NONE', #771, #2573, #6820, .T. ) ;
#4500 = DIRECTION ( 'NONE',  ( -0.000000000000000000, -0.000000000000000000, 1.000000000000000000 ) ) ;
#4501 = CARTESIAN_POINT ( 'NONE',  ( 25.00000000000000000, 0.000000000000000000, 2.055000000000000160 ) ) ;
#4502 = VECTOR ( 'NONE', #5373, 1000.000000000000000 ) ;
#4503 = ORIENTED_EDGE ( 'NONE', *, *, #6775, .F. ) ;
#4504 =( NAMED_UNIT ( * ) SI_UNIT ( $, .STERADIAN. ) SOLID_ANGLE_UNIT ( ) );
#4505 = CARTESIAN_POINT ( 'NONE',  ( -4.000000000000000000, 0.7924765000094600165, -0.05906175389889745803 ) ) ;
#4506 = ORIENTED_EDGE ( 'NONE', *, *, #6988, .F. ) ;
#4507 = CIRCLE ( 'NONE', #4092, 2.041999999999999815 ) ;
#4508 = DIRECTION ( 'NONE',  ( -0.9284766908852593037, 0.000000000000000000, -0.3713906763541036660 ) ) ;
#4509 = CARTESIAN_POINT ( 'NONE',  ( 5.000000000000000000, -5.000000000000000000, 140.0000000000000000 ) ) ;
#4510 = EDGE_CURVE ( 'NONE', #8486, #6933, #8530, .T. ) ;
#4511 = CARTESIAN_POINT ( 'NONE',  ( -4.000000000000000000, -1.942223658245633811, -0.3516579909967644246 ) ) ;
#4512 = EDGE_LOOP ( 'NONE', ( #1163, #7397, #84, #3820 ) ) ;
#4513 = DIRECTION ( 'NONE',  ( 0.000000000000000000, 0.000000000000000000, 1.000000000000000000 ) ) ;
#4514 = DIRECTION ( 'NONE',  ( 0.000000000000000000, 0.000000000000000000, -1.000000000000000000 ) ) ;
#4515 = VERTEX_POINT ( 'NONE', #8008 ) ;
#4516 = ORIENTED_EDGE ( 'NONE', *, *, #4059, .T. ) ;
#4517 = CARTESIAN_POINT ( 'NONE',  ( 82.99999999999998579, -4.999999999999998224, 140.0000000000000000 ) ) ;
#4518 = FACE_OUTER_BOUND ( 'NONE', #3092, .T. ) ;
#4519 =( REPRESENTATION_RELATIONSHIP ('NONE','NONE', #3312, #4754 ) REPRESENTATION_RELATIONSHIP_WITH_TRANSFORMATION ( #589 )SHAPE_REPRESENTATION_RELATIONSHIP( ) );
#4520 = DIRECTION ( 'NONE',  ( -1.734723475976807587E-16, 1.000000000000000000, 0.000000000000000000 ) ) ;
#4521 = DIRECTION ( 'NONE',  ( -1.000000000000000000, 0.000000000000000000, -0.000000000000000000 ) ) ;
#4522 = VERTEX_POINT ( 'NONE', #7252 ) ;
#4523 = AXIS2_PLACEMENT_3D ( 'NONE', #7009, #1135, #2535 ) ;
#4524 = ORIENTED_EDGE ( 'NONE', *, *, #172, .F. ) ;
#4525 = PLANE ( 'NONE',  #2412 ) ;
#4526 = AXIS2_PLACEMENT_3D ( 'NONE', #5546, #3768, #5068 ) ;
#4527 = AXIS2_PLACEMENT_3D ( 'NONE', #7610, #240, #1689 ) ;
#4528 = CARTESIAN_POINT ( 'NONE',  ( 0.2500000000000002220, 0.000000000000000000, 4.000000000000000000 ) ) ;
#4529 = CARTESIAN_POINT ( 'NONE',  ( 0.000000000000000000, 0.000000000000000000, -5.000000000000000888 ) ) ;
#4530 = CARTESIAN_POINT ( 'NONE',  ( 5.000000000000000000, -5.000000000000000000, 34.00000000000000711 ) ) ;
#4531 = SURFACE_STYLE_USAGE ( .BOTH. , #5148 ) ;
#4532 = AXIS2_PLACEMENT_3D ( 'NONE', #583, #50, #626 ) ;
#4533 = AXIS2_PLACEMENT_3D ( 'NONE', #122, #6746, #1969 ) ;
#4534 =( LENGTH_UNIT ( ) NAMED_UNIT ( * ) SI_UNIT ( .MILLI., .METRE. ) );
#4535 = DIRECTION ( 'NONE',  ( 0.000000000000000000, 0.000000000000000000, 1.000000000000000000 ) ) ;
#4536 = ADVANCED_FACE ( 'NONE', ( #2609, #601, #5290, #8574, #4554, #4002, #5210 ), #5983, .F. ) ;
#4537 = DIRECTION ( 'NONE',  ( 1.000000000000000000, -1.734723475976806848E-16, 0.000000000000000000 ) ) ;
#4538 = EDGE_CURVE ( 'NONE', #2983, #2875, #3829, .T. ) ;
#4539 = EDGE_CURVE ( 'NONE', #5788, #1754, #7916, .T. ) ;
#4540 = CYLINDRICAL_SURFACE ( 'NONE', #111, 2.649999999999985700 ) ;
#4541 = CARTESIAN_POINT ( 'NONE',  ( 5.000000000000001776, 140.0000000000000000, 15.00000000000000355 ) ) ;
#4542 = ORIENTED_EDGE ( 'NONE', *, *, #745, .F. ) ;
#4543 =( NAMED_UNIT ( * ) PLANE_ANGLE_UNIT ( ) SI_UNIT ( $, .RADIAN. ) );
#4544 = CARTESIAN_POINT ( 'NONE',  ( 2.500000000000000000, -1.178949249685213863, 2.042000000000002924 ) ) ;
#4545 = ORIENTED_EDGE ( 'NONE', *, *, #2927, .F. ) ;
#4546 = DIRECTION ( 'NONE',  ( 1.000000000000000000, 0.000000000000000000, 0.000000000000000000 ) ) ;
#4547 = DIRECTION ( 'NONE',  ( 0.000000000000000000, 1.000000000000000000, 0.000000000000000000 ) ) ;
#4548 = PRODUCT_DEFINITION_CONTEXT ( 'detailed design', #2860, 'design' ) ;
#4549 = CARTESIAN_POINT ( 'NONE',  ( -30.00000000000002842, -20.00000000000000000, 180.0000000000000284 ) ) ;
#4550 = ORIENTED_EDGE ( 'NONE', *, *, #5176, .T. ) ;
#4551 = FACE_OUTER_BOUND ( 'NONE', #3536, .T. ) ;
#4552 = ADVANCED_FACE ( 'NONE', ( #8490 ), #6642, .T. ) ;
#4553 = CARTESIAN_POINT ( 'NONE',  ( 263.9999999999999432, -30.00000000000000000, -51.43142504031547446 ) ) ;
#4554 = FACE_BOUND ( 'NONE', #4989, .T. ) ;
#4555 = ORIENTED_EDGE ( 'NONE', *, *, #3596, .F. ) ;
#4556 = EDGE_LOOP ( 'NONE', ( #6226, #5462, #8420, #3767 ) ) ;
#4557 = CARTESIAN_POINT ( 'NONE',  ( 5.000000000000004441, 0.000000000000000000, 0.000000000000000000 ) ) ;
#4558 = CARTESIAN_POINT ( 'NONE',  ( 347.0000000000000000, -4.999999999999998224, 139.9990000000000236 ) ) ;
#4559 = CARTESIAN_POINT ( 'NONE',  ( 2.000000000000005329, -3.464101615137751722, 0.000000000000000000 ) ) ;
#4560 = AXIS2_PLACEMENT_3D ( 'NONE', #5821, #2414, #391 ) ;
#4561 = LINE ( 'NONE', #3881, #5123 ) ;
#4562 = ORIENTED_EDGE ( 'NONE', *, *, #2177, .F. ) ;
#4563 = EDGE_CURVE ( 'NONE', #806, #2303, #1143, .T. ) ;
#4564 =( NAMED_UNIT ( * ) PLANE_ANGLE_UNIT ( ) SI_UNIT ( $, .RADIAN. ) );
#4565 = EDGE_CURVE ( 'NONE', #133, #8215, #3786, .T. ) ;
#4566 = EDGE_LOOP ( 'NONE', ( #5291, #254, #5810, #7965 ) ) ;
#4567 = DIRECTION ( 'NONE',  ( 0.000000000000000000, 0.000000000000000000, -1.000000000000000000 ) ) ;
#4568 = ADVANCED_FACE ( 'NONE', ( #4596 ), #5855, .F. ) ;
#4569 = AXIS2_PLACEMENT_3D ( 'NONE', #4304, #1697, #4344 ) ;
#4570 = CARTESIAN_POINT ( 'NONE',  ( 0.000000000000000000, 0.000000000000000000, 0.000000000000000000 ) ) ;
#4571 = DIRECTION ( 'NONE',  ( 1.000000000000000000, -1.734723475976806848E-16, 0.000000000000000000 ) ) ;
#4572 = ORIENTED_EDGE ( 'NONE', *, *, #1844, .T. ) ;
#4573 = CARTESIAN_POINT ( 'NONE',  ( 20.00000000000000000, 135.0000000000000000, 0.000000000000000000 ) ) ;
#4574 = DIRECTION ( 'NONE',  ( -1.000000000000000000, 0.000000000000000000, 0.000000000000000000 ) ) ;
#4575 = CIRCLE ( 'NONE', #4714, 10.00000000000000000 ) ;
#4576 = CARTESIAN_POINT ( 'NONE',  ( 0.000000000000000000, 0.000000000000000000, -115.0000000000000000 ) ) ;
#4577 = CARTESIAN_POINT ( 'NONE',  ( 10.00000000000000000, 0.000000000000000000, 120.0000000000000284 ) ) ;
#4578 = DIRECTION ( 'NONE',  ( 0.000000000000000000, 1.000000000000000000, 0.000000000000000000 ) ) ;
#4579 = VECTOR ( 'NONE', #3499, 1000.000000000000000 ) ;
#4580 = EDGE_CURVE ( 'NONE', #428, #7903, #5940, .T. ) ;
#4581 = PLANE ( 'NONE',  #3751 ) ;
#4582 = CARTESIAN_POINT ( 'NONE',  ( 136.6666666666666288, -25.00000000000000000, 162.5000000000000853 ) ) ;
#4583 = CARTESIAN_POINT ( 'NONE',  ( 434.9999999999999432, -4.999999999999998224, 140.0000000000000000 ) ) ;
#4584 = ORIENTED_EDGE ( 'NONE', *, *, #3194, .T. ) ;
#4585 = FILL_AREA_STYLE_COLOUR ( '', #4497 ) ;
#4586 = CARTESIAN_POINT ( 'NONE',  ( -4.000000000000000888, 1.563622288139195238, -0.2253451193528307472 ) ) ;
#4587 = ITEM_DEFINED_TRANSFORMATION ( 'NONE', 'NONE', #6278,  #594 ) ;
#4588 = VECTOR ( 'NONE', #4809, 1000.000000000000000 ) ;
#4589 = ORIENTED_EDGE ( 'NONE', *, *, #2295, .T. ) ;
#4590 = DIRECTION ( 'NONE',  ( -0.000000000000000000, 1.000000000000000000, 1.224646799147353207E-16 ) ) ;
#4591 = ADVANCED_FACE ( 'NONE', ( #2650 ), #7962, .F. ) ;
#4592 = CARTESIAN_POINT ( 'NONE',  ( -5.000000000000000000, -5.000000000000000000, 140.0000000000000000 ) ) ;
#4593 = DIRECTION ( 'NONE',  ( 0.000000000000000000, 0.000000000000000000, 1.000000000000000000 ) ) ;
#4594 = EDGE_LOOP ( 'NONE', ( #7105, #7687, #7387, #1185 ) ) ;
#4595 = CARTESIAN_POINT ( 'NONE',  ( 5.000000000000000000, -5.000000000000000000, 148.0000000000000284 ) ) ;
#4596 = FACE_OUTER_BOUND ( 'NONE', #3796, .T. ) ;
#4597 = ORIENTED_EDGE ( 'NONE', *, *, #1456, .F. ) ;
#4598 = ORIENTED_EDGE ( 'NONE', *, *, #5363, .F. ) ;
#4599 = COLOUR_RGB ( '',0.8941176470588234615, 0.8941176470588234615, 0.8941176470588234615 ) ;
#4600 = CARTESIAN_POINT ( 'NONE',  ( -4.000000000000000000, 2.309401076758498483, -3.433295621305379353 ) ) ;
#4601 = CARTESIAN_POINT ( 'NONE',  ( 0.000000000000000000, 0.000000000000000000, -27.99999999999999645 ) ) ;
#4602 = CARTESIAN_POINT ( 'NONE',  ( 4.000000000000000000, 0.8378280264232961239, -3.220590601395640018 ) ) ;
#4603 = VECTOR ( 'NONE', #3977, 1000.000000000000000 ) ;
#4604 = LINE ( 'NONE', #6563, #5396 ) ;
#4605 = EDGE_LOOP ( 'NONE', ( #7321, #7643 ) ) ;
#4606 = PRESENTATION_LAYER_ASSIGNMENT (  '', '', ( #2543 ) ) ;
#4607 = ORIENTED_EDGE ( 'NONE', *, *, #1090, .T. ) ;
#4608 = DIRECTION ( 'NONE',  ( 0.000000000000000000, 0.000000000000000000, -1.000000000000000000 ) ) ;
#4609 = CARTESIAN_POINT ( 'NONE',  ( -10.00000000000000000, 1.224646799147353059E-15, 140.0000000000000000 ) ) ;
#4610 = AXIS2_PLACEMENT_3D ( 'NONE', #3451, #127, #2797 ) ;
#4611 = EDGE_CURVE ( 'NONE', #2181, #1089, #6815, .T. ) ;
#4612 = EDGE_CURVE ( 'NONE', #6761, #5082, #4819, .T. ) ;
#4613 = AXIS2_PLACEMENT_3D ( 'NONE', #5013, #1673, #4321 ) ;
#4614 = CARTESIAN_POINT ( 'NONE',  ( -30.00000000000000000, -15.00000000000000000, 145.0000000000000284 ) ) ;
#4615 = FACE_OUTER_BOUND ( 'NONE', #4297, .T. ) ;
#4616 = ORIENTED_EDGE ( 'NONE', *, *, #2468, .T. ) ;
#4617 = CARTESIAN_POINT ( 'NONE',  ( 93.00000000000000000, 5.000000000000000000, 145.0000000000000284 ) ) ;
#4618 = FACE_OUTER_BOUND ( 'NONE', #6283, .T. ) ;
#4619 = VECTOR ( 'NONE', #747, 1000.000000000000000 ) ;
#4620 = CARTESIAN_POINT ( 'NONE',  ( -30.00000000000002842, -24.99999999999980105, -200.0000000000000000 ) ) ;
#4621 = AXIS2_PLACEMENT_3D ( 'NONE', #4917, #7442, #4097 ) ;
#4622 = DIRECTION ( 'NONE',  ( 0.000000000000000000, 0.000000000000000000, 1.000000000000000000 ) ) ;
#4623 = CARTESIAN_POINT ( 'NONE',  ( -5.000000000000001776, 5.000000000000001776, 42.00000000000000711 ) ) ;
#4624 = AXIS2_PLACEMENT_3D ( 'NONE', #1174, #7834, #3345 ) ;
#4625 = CARTESIAN_POINT ( 'NONE',  ( 2.059999999999998721, 0.000000000000000000, -0.3080913168122742518 ) ) ;
#4626 = EDGE_CURVE ( 'NONE', #4892, #6564, #5423, .T. ) ;
#4627 = DIRECTION ( 'NONE',  ( 0.000000000000000000, 1.000000000000000000, 0.000000000000000000 ) ) ;
#4628 = CARTESIAN_POINT ( 'NONE',  ( -5.000000000000000000, -5.000000000000000000, 148.0000000000000284 ) ) ;
#4629 = MECHANICAL_DESIGN_GEOMETRIC_PRESENTATION_REPRESENTATION (  '', ( #5185 ), #2005 ) ;
#4630 = ORIENTED_EDGE ( 'NONE', *, *, #5284, .T. ) ;
#4631 = EDGE_LOOP ( 'NONE', ( #6769, #3267, #1001, #4691 ) ) ;
#4632 = ORIENTED_EDGE ( 'NONE', *, *, #2503, .T. ) ;
#4633 =( REPRESENTATION_RELATIONSHIP ('NONE','NONE', #3312, #1479 ) REPRESENTATION_RELATIONSHIP_WITH_TRANSFORMATION ( #418 )SHAPE_REPRESENTATION_RELATIONSHIP( ) );
#4634 = PLANE ( 'NONE',  #2301 ) ;
#4635 = CARTESIAN_POINT ( 'NONE',  ( 5.000000000000000000, 5.000000000000000000, -71.99999999999998579 ) ) ;
#4636 = CIRCLE ( 'NONE', #1302, 20.00000000000000000 ) ;
#4637 = DIRECTION ( 'NONE',  ( 1.000000000000000000, 1.734723475976806848E-16, -0.000000000000000000 ) ) ;
#4638 = ORIENTED_EDGE ( 'NONE', *, *, #2409, .F. ) ;
#4639 = CARTESIAN_POINT ( 'NONE',  ( 5.000000000000000000, 5.000000000000000000, 148.0000000000000284 ) ) ;
#4640 = AXIS2_PLACEMENT_3D ( 'NONE', #4558, #2087, #692 ) ;
#4641 = DIRECTION ( 'NONE',  ( 1.000000000000000000, 0.000000000000000000, 0.000000000000000000 ) ) ;
#4642 = DIRECTION ( 'NONE',  ( -0.8126014203817149006, 1.665334536937734318E-16, -0.5828198105706593468 ) ) ;
#4643 = CARTESIAN_POINT ( 'NONE',  ( -0.3198814748697807464, -4.434118497892185040, -0.3507732604232532969 ) ) ;
#4644 = ORIENTED_EDGE ( 'NONE', *, *, #1300, .F. ) ;
#4645 = ORIENTED_EDGE ( 'NONE', *, *, #3925, .F. ) ;
#4646 = CARTESIAN_POINT ( 'NONE',  ( -4.000000000000000000, -2.309401076758512694, -3.433295621305382461 ) ) ;
#4647 = DIRECTION ( 'NONE',  ( 1.000000000000000000, -1.734723475976806848E-16, 0.000000000000000000 ) ) ;
#4648 = ADVANCED_FACE ( 'NONE', ( #8097 ), #2818, .F. ) ;
#4649 = CARTESIAN_POINT ( 'NONE',  ( 3.999999999999998224, 2.472263674411418588, -3.687027874309861897 ) ) ;
#4650 = DIRECTION ( 'NONE',  ( -0.9396926207859138680, 0.000000000000000000, -0.3420201433256536139 ) ) ;
#4651 = ORIENTED_EDGE ( 'NONE', *, *, #1589, .F. ) ;
#4652 = ADVANCED_FACE ( 'NONE', ( #5466 ), #7347, .F. ) ;
#4653 = EDGE_LOOP ( 'NONE', ( #5843, #448, #8194, #7167 ) ) ;
#4654 = MANIFOLD_SOLID_BREP ( 'M5 Clearance Hole1', #8448 ) ;
#4655 = VECTOR ( 'NONE', #5162, 1000.000000000000000 ) ;
#4656 = FACE_OUTER_BOUND ( 'NONE', #5777, .T. ) ;
#4657 = DIRECTION ( 'NONE',  ( -0.000000000000000000, -0.000000000000000000, 1.000000000000000000 ) ) ;
#4658 = VERTEX_POINT ( 'NONE', #6681 ) ;
#4659 = LINE ( 'NONE', #6049, #2910 ) ;
#4660 = EDGE_CURVE ( 'NONE', #7555, #7704, #7431, .T. ) ;
#4661 = LINE ( 'NONE', #1937, #7826 ) ;
#4663 = AXIS2_PLACEMENT_3D ( 'NONE', #4335, #414, #5679 ) ;
#4662 = B_SPLINE_CURVE_WITH_KNOTS ( 'NONE', 3,
 ( #7709, #5038, #5646, #8319, #7234 ),
 .UNSPECIFIED., .F., .F.,
 ( 4, 1, 4 ),
 ( 0.000000000000000000, 0.002309401076758505356, 0.004618802153517010713 ),
 .UNSPECIFIED. ) ;
#4664 = CARTESIAN_POINT ( 'NONE',  ( -30.00000000000002842, -20.00000000000000000, 200.0000000000000000 ) ) ;
#4665 = CARTESIAN_POINT ( 'NONE',  ( 259.0000000000000000, -4.999999999999998224, 145.0000000000000284 ) ) ;
#4666 = DIRECTION ( 'NONE',  ( -0.000000000000000000, -0.000000000000000000, 1.000000000000000000 ) ) ;
#4667 = VECTOR ( 'NONE', #5452, 1000.000000000000000 ) ;
#4668 = DIRECTION ( 'NONE',  ( 1.000000000000000000, 0.000000000000000000, 0.000000000000000000 ) ) ;
#4669 = DIRECTION ( 'NONE',  ( -0.000000000000000000, -1.000000000000000000, -0.000000000000000000 ) ) ;
#4670 = VECTOR ( 'NONE', #4052, 1000.000000000000000 ) ;
#4671 = ORIENTED_EDGE ( 'NONE', *, *, #7823, .T. ) ;
#4672 = FILL_AREA_STYLE_COLOUR ( '', #1861 ) ;
#4673 = VERTEX_POINT ( 'NONE', #6730 ) ;
#4674 = CONTEXT_DEPENDENT_SHAPE_REPRESENTATION ( #1695, #4275 ) ;
#4675 = UNCERTAINTY_MEASURE_WITH_UNIT (LENGTH_MEASURE( 1.000000000000000082E-05 ), #6248, 'distance_accuracy_value', 'NONE');
#4676 = ORIENTED_EDGE ( 'NONE', *, *, #7528, .T. ) ;
#4677 = CARTESIAN_POINT ( 'NONE',  ( 5.000000000000000888, 0.000000000000000000, 0.000000000000000000 ) ) ;
#4678 = CARTESIAN_POINT ( 'NONE',  ( -4.000000000000000000, -2.309401076758512694, -3.433295621305382461 ) ) ;
#4679 = COLOUR_RGB ( '',0.8941176470588234615, 0.8941176470588234615, 0.8941176470588234615 ) ;
#4680 = AXIS2_PLACEMENT_3D ( 'NONE', #8439, #2517, #2562 ) ;
#4681 = PRODUCT_DEFINITION_SHAPE ( 'NONE', 'NONE',  #8608 ) ;
#4682 = VERTEX_POINT ( 'NONE', #3476 ) ;
#4683 = DIRECTION ( 'NONE',  ( 0.000000000000000000, 0.000000000000000000, -1.000000000000000000 ) ) ;
#4684 = ORIENTED_EDGE ( 'NONE', *, *, #8314, .F. ) ;
#4685 = LINE ( 'NONE', #5898, #3801 ) ;
#4686 = MANIFOLD_SOLID_BREP ( 'Boss-Extrude4', #6195 ) ;
#4687 = DIRECTION ( 'NONE',  ( 0.000000000000000000, 0.000000000000000000, 1.000000000000000000 ) ) ;
#4688 = SHAPE_DEFINITION_REPRESENTATION ( #1345, #638 ) ;
#4689 =( LENGTH_UNIT ( ) NAMED_UNIT ( * ) SI_UNIT ( .MILLI., .METRE. ) );
#4690 = ORIENTED_EDGE ( 'NONE', *, *, #8088, .T. ) ;
#4691 = ORIENTED_EDGE ( 'NONE', *, *, #2265, .T. ) ;
#4692 = DIRECTION ( 'NONE',  ( 1.000000000000000000, 0.000000000000000000, 0.000000000000000000 ) ) ;
#4693 = FACE_OUTER_BOUND ( 'NONE', #6437, .T. ) ;
#4694 = ADVANCED_FACE ( 'NONE', ( #6457 ), #5552, .F. ) ;
#4695 = CARTESIAN_POINT ( 'NONE',  ( 82.99999999999998579, 5.000000000000001776, 139.9990000000000236 ) ) ;
#4696 = LINE ( 'NONE', #3399, #3734 ) ;
#4697 = VERTEX_POINT ( 'NONE', #8429 ) ;
#4698 = ADVANCED_FACE ( 'NONE', ( #950 ), #4904, .F. ) ;
#4699 = SURFACE_STYLE_FILL_AREA ( #8065 ) ;
#4700 = ORIENTED_EDGE ( 'NONE', *, *, #1301, .T. ) ;
#4701 = LINE ( 'NONE', #1968, #7969 ) ;
#4702 = EDGE_CURVE ( 'NONE', #5985, #6827, #3853, .T. ) ;
#4703 = MANIFOLD_SOLID_BREP ( 'Boss-Extrude4', #2471 ) ;
#4704 = EDGE_CURVE ( 'NONE', #7348, #7567, #3601, .T. ) ;
#4705 = AXIS2_PLACEMENT_3D ( 'NONE', #3448, #2794, #8117 ) ;
#4706 = SHAPE_REPRESENTATION ( 'roller axis assy_r6', ( #594 ), #8234 ) ;
#4707 = LINE ( 'NONE', #5398, #6343 ) ;
#4708 = DIRECTION ( 'NONE',  ( 0.000000000000000000, 1.000000000000000000, 0.000000000000000000 ) ) ;
#4709 = ORIENTED_EDGE ( 'NONE', *, *, #3577, .T. ) ;
#4710 = FACE_OUTER_BOUND ( 'NONE', #2482, .T. ) ;
#4711 = AXIS2_PLACEMENT_3D ( 'NONE', #5970, #8038, #4668 ) ;
#4712 =( NAMED_UNIT ( * ) SI_UNIT ( $, .STERADIAN. ) SOLID_ANGLE_UNIT ( ) );
#4713 = PLANE ( 'NONE',  #7399 ) ;
#4714 = AXIS2_PLACEMENT_3D ( 'NONE', #4105, #7936, #6575 ) ;
#4715 = CARTESIAN_POINT ( 'NONE',  ( 0.000000000000000000, 0.000000000000000000, 120.0000000000000142 ) ) ;
#4716 = CARTESIAN_POINT ( 'NONE',  ( -5.000000000000000000, -5.000000000000000000, -0.9999999999999940048 ) ) ;
#4717 = CARTESIAN_POINT ( 'NONE',  ( 4.000000000000000000, -2.309401076758516691, -0.4999999999999995559 ) ) ;
#4718 = ORIENTED_EDGE ( 'NONE', *, *, #7913, .F. ) ;
#4719 = EDGE_LOOP ( 'NONE', ( #631, #8043, #2706, #6105 ) ) ;
#4720 = ORIENTED_EDGE ( 'NONE', *, *, #1538, .F. ) ;
#4721 = CYLINDRICAL_SURFACE ( 'NONE', #2009, 2.100000000000000089 ) ;
#4722 = AXIS2_PLACEMENT_3D ( 'NONE', #2719, #8037, #5273 ) ;
#4723 = SURFACE_STYLE_FILL_AREA ( #1505 ) ;
#4724 = EDGE_CURVE ( 'NONE', #628, #3262, #8511, .T. ) ;
#4725 = ADVANCED_FACE ( 'NONE', ( #5150 ), #441, .T. ) ;
#4726 = VERTEX_POINT ( 'NONE', #575 ) ;
#4727 = LINE ( 'NONE', #2567, #2463 ) ;
#4728 = ORIENTED_EDGE ( 'NONE', *, *, #2524, .F. ) ;
#4729 = DIRECTION ( 'NONE',  ( -1.000000000000000000, 0.000000000000000000, 0.000000000000000000 ) ) ;
#4730 = ADVANCED_FACE ( 'NONE', ( #3199 ), #5833, .F. ) ;
#4731 = DIRECTION ( 'NONE',  ( 0.000000000000000000, 0.000000000000000000, 1.000000000000000000 ) ) ;
#4732 = APPLICATION_PROTOCOL_DEFINITION ( 'draft international standard', 'automotive_design', 1998, #2313 ) ;
#4733 = SURFACE_STYLE_USAGE ( .BOTH. , #817 ) ;
#4734 = ORIENTED_EDGE ( 'NONE', *, *, #3798, .F. ) ;
#4735 = VERTEX_POINT ( 'NONE', #3892 ) ;
#4736 = DIRECTION ( 'NONE',  ( 0.000000000000000000, 0.000000000000000000, 1.000000000000000000 ) ) ;
#4737 = FACE_OUTER_BOUND ( 'NONE', #5942, .T. ) ;
#4738 = ADVANCED_FACE ( 'NONE', ( #1601 ), #7193, .F. ) ;
#4739 = CARTESIAN_POINT ( 'NONE',  ( 170.9999999999999716, -4.999999999999998224, 140.0000000000000000 ) ) ;
#4740 = DIRECTION ( 'NONE',  ( 0.000000000000000000, 0.000000000000000000, 1.000000000000000000 ) ) ;
#4741 = EDGE_CURVE ( 'NONE', #3015, #5505, #8269, .T. ) ;
#4742 = ORIENTED_EDGE ( 'NONE', *, *, #1118, .F. ) ;
#4743 =( NAMED_UNIT ( * ) SI_UNIT ( $, .STERADIAN. ) SOLID_ANGLE_UNIT ( ) );
#4744 = DIRECTION ( 'NONE',  ( 1.000000000000000000, 0.000000000000000000, 0.000000000000000000 ) ) ;
#4745 = ORIENTED_EDGE ( 'NONE', *, *, #3379, .T. ) ;
#4746 = LINE ( 'NONE', #3530, #6847 ) ;
#4747 = DIRECTION ( 'NONE',  ( 0.000000000000000000, 1.000000000000000000, 0.000000000000000000 ) ) ;
#4748 = LINE ( 'NONE', #6532, #2486 ) ;
#4749 = ORIENTED_EDGE ( 'NONE', *, *, #7064, .F. ) ;
#4750 = CARTESIAN_POINT ( 'NONE',  ( 0.000000000000000000, 0.000000000000000000, -5.000000000000000000 ) ) ;
#4751 = ORIENTED_EDGE ( 'NONE', *, *, #7174, .T. ) ;
#4752 = DIRECTION ( 'NONE',  ( 0.000000000000000000, 0.000000000000000000, 1.000000000000000000 ) ) ;
#4753 =( GEOMETRIC_REPRESENTATION_CONTEXT ( 3 ) GLOBAL_UNCERTAINTY_ASSIGNED_CONTEXT ( ( #3322 ) ) GLOBAL_UNIT_ASSIGNED_CONTEXT ( ( #4689, #6773, #4085 ) ) REPRESENTATION_CONTEXT ( 'NONE', 'WORKASPACE' ) );
#4754 = SHAPE_REPRESENTATION ( 'hex flange nut gradea_iso_ISO - 4161 - M5 - N', ( #594 ), #750 ) ;
#4755 = LINE ( 'NONE', #2067, #6558 ) ;
#4756 = VECTOR ( 'NONE', #6797, 1000.000000000000000 ) ;
#4757 = MANIFOLD_SOLID_BREP ( 'Boss-Extrude4', #7600 ) ;
#4758 = CARTESIAN_POINT ( 'NONE',  ( -5.000000000000000000, -5.000000000000000000, -105.9999999999999858 ) ) ;
#4759 = EDGE_CURVE ( 'NONE', #951, #4853, #7278, .T. ) ;
#4760 = LINE ( 'NONE', #1451, #6373 ) ;
#4761 = CARTESIAN_POINT ( 'NONE',  ( 5.560781378645573980, 6.809993116116507654E-16, -4.000000000000000000 ) ) ;
#4762 = ORIENTED_EDGE ( 'NONE', *, *, #3224, .T. ) ;
#4763 = ADVANCED_FACE ( 'NONE', ( #7066 ), #6751, .F. ) ;
#4764 = AXIS2_PLACEMENT_3D ( 'NONE', #142, #6108, #6726 ) ;
#4765 = VERTEX_POINT ( 'NONE', #5403 ) ;
#4766 = ORIENTED_EDGE ( 'NONE', *, *, #1952, .T. ) ;
#4767 = CIRCLE ( 'NONE', #5311, 10.00000000000000000 ) ;
#4768 = DIRECTION ( 'NONE',  ( -0.000000000000000000, 1.000000000000000000, -0.000000000000000000 ) ) ;
#4769 = AXIS2_PLACEMENT_3D ( 'NONE', #7669, #1705, #6441 ) ;
#4770 = LINE ( 'NONE', #7422, #4076 ) ;
#4771 = VECTOR ( 'NONE', #1125, 1000.000000000000000 ) ;
#4772 =( GEOMETRIC_REPRESENTATION_CONTEXT ( 3 ) GLOBAL_UNCERTAINTY_ASSIGNED_CONTEXT ( ( #3376 ) ) GLOBAL_UNIT_ASSIGNED_CONTEXT ( ( #1161, #7496, #3372 ) ) REPRESENTATION_CONTEXT ( 'NONE', 'WORKASPACE' ) );
#4773 = VERTEX_POINT ( 'NONE', #3410 ) ;
#4774 = LINE ( 'NONE', #7512, #2325 ) ;
#4775 = VERTEX_POINT ( 'NONE', #5231 ) ;
#4776 = DIRECTION ( 'NONE',  ( -0.000000000000000000, -0.000000000000000000, 1.000000000000000000 ) ) ;
#4777 = DIRECTION ( 'NONE',  ( -0.000000000000000000, -0.000000000000000000, 1.000000000000000000 ) ) ;
#4778 = ITEM_DEFINED_TRANSFORMATION ( 'NONE', 'NONE', #5018,  #594 ) ;
#4779 = ORIENTED_EDGE ( 'NONE', *, *, #3375, .F. ) ;
#4780 = VERTEX_POINT ( 'NONE', #7230 ) ;
#4781 = ADVANCED_FACE ( 'NONE', ( #800 ), #6050, .T. ) ;
#4782 = DIRECTION ( 'NONE',  ( 0.000000000000000000, 0.000000000000000000, 1.000000000000000000 ) ) ;
#4783 = CARTESIAN_POINT ( 'NONE',  ( -3.974344831685191280E-13, 4.796734841935104576, -3.721909803043223608 ) ) ;
#4784 = CIRCLE ( 'NONE', #1180, 2.041999999999999815 ) ;
#4785 = DIRECTION ( 'NONE',  ( -0.000000000000000000, -0.000000000000000000, 1.000000000000000000 ) ) ;
#4786 = LINE ( 'NONE', #827, #5539 ) ;
#4787 = ORIENTED_EDGE ( 'NONE', *, *, #7720, .F. ) ;
#4788 = PLANE ( 'NONE',  #5727 ) ;
#4789 = VERTEX_POINT ( 'NONE', #5269 ) ;
#4790 = ORIENTED_EDGE ( 'NONE', *, *, #5724, .T. ) ;
#4791 = CARTESIAN_POINT ( 'NONE',  ( -3.355112389629170799, 2.681727112203152963, -0.2256878752776689534 ) ) ;
#4792 = PRODUCT_DEFINITION ( 'UNKNOWN', '', #300, #7866 ) ;
#4793 = EDGE_CURVE ( 'NONE', #3710, #8068, #2759, .T. ) ;
#4794 = DIRECTION ( 'NONE',  ( -1.000000000000000000, 0.000000000000000000, -0.000000000000000000 ) ) ;
#4795 = FACE_BOUND ( 'NONE', #3400, .T. ) ;
#4796 = EDGE_LOOP ( 'NONE', ( #7806, #4176 ) ) ;
#4797 = DIRECTION ( 'NONE',  ( -1.000000000000000000, 0.000000000000000000, 0.000000000000000000 ) ) ;
#4798 = DIRECTION ( 'NONE',  ( -0.000000000000000000, -0.000000000000000000, 1.000000000000000000 ) ) ;
#4799 = CARTESIAN_POINT ( 'NONE',  ( 53.33333333333330017, -20.00000000000000000, 162.5000000000000853 ) ) ;
#4800 =( REPRESENTATION_RELATIONSHIP ('NONE','NONE', #3312, #4754 ) REPRESENTATION_RELATIONSHIP_WITH_TRANSFORMATION ( #6631 )SHAPE_REPRESENTATION_RELATIONSHIP( ) );
#4801 = FACE_OUTER_BOUND ( 'NONE', #6258, .T. ) ;
#4802 = CARTESIAN_POINT ( 'NONE',  ( 219.9999999999999716, -20.00000000000000000, 159.8500000000001080 ) ) ;
#4803 =( NAMED_UNIT ( * ) PLANE_ANGLE_UNIT ( ) SI_UNIT ( $, .RADIAN. ) );
#4804 = ORIENTED_EDGE ( 'NONE', *, *, #1889, .T. ) ;
#4805 = CIRCLE ( 'NONE', #6888, 2.700000000000001066 ) ;
#4806 = ORIENTED_EDGE ( 'NONE', *, *, #7932, .T. ) ;
#4807 = EDGE_CURVE ( 'NONE', #7011, #5482, #4661, .T. ) ;
#4808 = ORIENTED_EDGE ( 'NONE', *, *, #5363, .T. ) ;
#4809 = DIRECTION ( 'NONE',  ( -0.000000000000000000, 1.000000000000000000, -0.000000000000000000 ) ) ;
#4810 = EDGE_CURVE ( 'NONE', #6932, #104, #1358, .T. ) ;
#4811 = ADVANCED_FACE ( 'NONE', ( #5357 ), #8078, .F. ) ;
#4812 = AXIS2_PLACEMENT_3D ( 'NONE', #6066, #100, #4201 ) ;
#4813 = VECTOR ( 'NONE', #8386, 1000.000000000000000 ) ;
#4814 = ORIENTED_EDGE ( 'NONE', *, *, #4330, .F. ) ;
#4815 = DIRECTION ( 'NONE',  ( 0.000000000000000000, -1.000000000000000000, 0.000000000000000000 ) ) ;
#4816 = ORIENTED_EDGE ( 'NONE', *, *, #2946, .F. ) ;
#4817 = LINE ( 'NONE', #3471, #8397 ) ;
#4818 = LINE ( 'NONE', #2082, #4258 ) ;
#4819 = LINE ( 'NONE', #8182, #1005 ) ;
#4820 = ORIENTED_EDGE ( 'NONE', *, *, #7346, .F. ) ;
#4821 = EDGE_LOOP ( 'NONE', ( #3250, #4262, #1793, #3747 ) ) ;
#4822 = AXIS2_PLACEMENT_3D ( 'NONE', #1587, #6096, #7372 ) ;
#4824 = VECTOR ( 'NONE', #345, 1000.000000000000000 ) ;
#4823 = CARTESIAN_POINT ( 'NONE',  ( -4.000000000000000000, -2.309401076758512694, -3.433295621305382461 ) ) ;
#4825 = DIRECTION ( 'NONE',  ( 0.000000000000000000, -0.5000000000000012212, -0.8660254037844380415 ) ) ;
#4826 = EDGE_CURVE ( 'NONE', #5500, #1781, #3096, .T. ) ;
#4827 = DIRECTION ( 'NONE',  ( 0.000000000000000000, -0.000000000000000000, 1.000000000000000000 ) ) ;
#4828 = EDGE_CURVE ( 'NONE', #563, #6157, #1271, .T. ) ;
#4829 = PRODUCT_DEFINITION_SHAPE ( 'NONE', 'NONE',  #8604 ) ;
#4830 = FACE_OUTER_BOUND ( 'NONE', #3724, .T. ) ;
#4831 = EDGE_LOOP ( 'NONE', ( #1078, #124, #7077, #2439, #4241, #429 ) ) ;
#4832 = DIRECTION ( 'NONE',  ( 0.000000000000000000, 0.000000000000000000, 1.000000000000000000 ) ) ;
#4833 = DIRECTION ( 'NONE',  ( -0.000000000000000000, -0.000000000000000000, 1.000000000000000000 ) ) ;
#4834 = ORIENTED_EDGE ( 'NONE', *, *, #8543, .T. ) ;
#4835 = ORIENTED_EDGE ( 'NONE', *, *, #3645, .T. ) ;
#4836 = DIRECTION ( 'NONE',  ( 0.000000000000000000, -0.5000000000000012212, -0.8660254037844380415 ) ) ;
#4837 = FACE_BOUND ( 'NONE', #382, .T. ) ;
#4838 = PLANE ( 'NONE',  #8033 ) ;
#4839 = ADVANCED_FACE ( 'NONE', ( #8035, #19 ), #2066, .F. ) ;
#4840 = FACE_BOUND ( 'NONE', #7994, .T. ) ;
#4841 = ORIENTED_EDGE ( 'NONE', *, *, #5439, .T. ) ;
#4842 = EDGE_CURVE ( 'NONE', #1565, #6692, #731, .T. ) ;
#4843 = DIRECTION ( 'NONE',  ( 0.000000000000000000, -0.000000000000000000, 1.000000000000000000 ) ) ;
#4844 = EDGE_CURVE ( 'NONE', #1160, #702, #6980, .T. ) ;
#4845 = CARTESIAN_POINT ( 'NONE',  ( 0.000000000000000000, 0.000000000000000000, 120.0000000000000284 ) ) ;
#4846 = CIRCLE ( 'NONE', #674, 20.00000000000000000 ) ;
#4847 = DIRECTION ( 'NONE',  ( 0.000000000000000000, 0.000000000000000000, -1.000000000000000000 ) ) ;
#4848 = DIRECTION ( 'NONE',  ( -1.000000000000000000, -0.000000000000000000, -0.000000000000000000 ) ) ;
#4849 = LINE ( 'NONE', #6189, #2371 ) ;
#4850 = CARTESIAN_POINT ( 'NONE',  ( 264.0000000000000000, -20.00000000000000000, -51.43142504031546025 ) ) ;
#4851 = AXIS2_PLACEMENT_3D ( 'NONE', #890, #1020, #4323 ) ;
#4852 = VERTEX_POINT ( 'NONE', #4620 ) ;
#4853 = VERTEX_POINT ( 'NONE', #1316 ) ;
#4854 = CARTESIAN_POINT ( 'NONE',  ( 2.855764796983346177, -2.970025579236428737, -0.09382832055446485575 ) ) ;
#4855 = AXIS2_PLACEMENT_3D ( 'NONE', #1492, #1622, #170 ) ;
#4856 = ORIENTED_EDGE ( 'NONE', *, *, #3190, .T. ) ;
#4857 = CARTESIAN_POINT ( 'NONE',  ( -5.000000000000001776, 5.000000000000001776, 34.00000000000000711 ) ) ;
#4858 = ORIENTED_EDGE ( 'NONE', *, *, #6565, .F. ) ;
#4859 = LINE ( 'NONE', #2119, #1577 ) ;
#4860 = DIRECTION ( 'NONE',  ( 0.000000000000000000, 0.000000000000000000, 1.000000000000000000 ) ) ;
#4861 = AXIS2_PLACEMENT_3D ( 'NONE', #1541, #2799, #6846 ) ;
#4862 = APPLICATION_PROTOCOL_DEFINITION ( 'draft international standard', 'automotive_design', 1998, #8095 ) ;
#4863 = SURFACE_STYLE_USAGE ( .BOTH. , #4041 ) ;
#4864 = ORIENTED_EDGE ( 'NONE', *, *, #288, .F. ) ;
#4865 = EDGE_CURVE ( 'NONE', #186, #819, #3978, .T. ) ;
#4866 = ORIENTED_EDGE ( 'NONE', *, *, #7672, .T. ) ;
#4867 = CARTESIAN_POINT ( 'NONE',  ( 5.000000000000000000, 5.000000000000000000, 148.0000000000000284 ) ) ;
#4868 = CYLINDRICAL_SURFACE ( 'NONE', #4909, 2.649999999999985700 ) ;
#4869 = AXIS2_PLACEMENT_3D ( 'NONE', #2449, #7047, #6392 ) ;
#4870 = CARTESIAN_POINT ( 'NONE',  ( -4.211140560182196957, -2.431303136016552013, -3.745885042887436178 ) ) ;
#4871 = CARTESIAN_POINT ( 'NONE',  ( 3.436319922986518449, -2.634841920959471562, -3.531542292954761741 ) ) ;
#4872 = EDGE_CURVE ( 'NONE', #6261, #6900, #6924, .T. ) ;
#4873 = ORIENTED_EDGE ( 'NONE', *, *, #8369, .F. ) ;
#4874 = B_SPLINE_CURVE_WITH_KNOTS ( 'NONE', 3,
 ( #2100, #703, #8593, #3450, #7890, #2624 ),
 .UNSPECIFIED., .F., .F.,
 ( 4, 2, 4 ),
 ( -3.640115492410698714E-06, 0.0002066546034006521879, 0.0004169493222937151081 ),
 .UNSPECIFIED. ) ;
#4875 = CARTESIAN_POINT ( 'NONE',  ( 357.0000000000000000, 5.000000000000000000, 140.0000000000000000 ) ) ;
#4876 = ORIENTED_EDGE ( 'NONE', *, *, #3382, .T. ) ;
#4877 = ORIENTED_EDGE ( 'NONE', *, *, #3228, .F. ) ;
#4878 = CARTESIAN_POINT ( 'NONE',  ( -3.680118525130244400, 2.494084732383327285, -0.3507732604232449702 ) ) ;
#4879 = DIRECTION ( 'NONE',  ( 1.000000000000000000, 1.734723475976806848E-16, -0.000000000000000000 ) ) ;
#4880 = CARTESIAN_POINT ( 'NONE',  ( 2.500000000000000888, 3.061616997868384127E-16, -4.974599999999998801 ) ) ;
#4881 = DIRECTION ( 'NONE',  ( -1.000000000000000000, 0.000000000000000000, 0.000000000000000000 ) ) ;
#4882 = ORIENTED_EDGE ( 'NONE', *, *, #6408, .F. ) ;
#4883 = DIRECTION ( 'NONE',  ( -1.000000000000000000, 0.000000000000000000, 0.000000000000000000 ) ) ;
#4884 = CARTESIAN_POINT ( 'NONE',  ( -5.000000000000001776, 5.000000000000001776, -0.9999999999999940048 ) ) ;
#4885 = EDGE_CURVE ( 'NONE', #7549, #989, #4199, .T. ) ;
#4886 = EDGE_CURVE ( 'NONE', #8169, #8541, #8519, .T. ) ;
#4887 = CARTESIAN_POINT ( 'NONE',  ( 82.99999999999998579, -4.999999999999998224, 140.0000000000000000 ) ) ;
#4888 = FACE_OUTER_BOUND ( 'NONE', #520, .T. ) ;
#4889 = CARTESIAN_POINT ( 'NONE',  ( 0.000000000000000000, 0.000000000000000000, -49.56854249492377562 ) ) ;
#4890 = CARTESIAN_POINT ( 'NONE',  ( 3.999999999999999112, -0.7890432684750902093, -0.04868663549882291247 ) ) ;
#4891 = AXIS2_PLACEMENT_3D ( 'NONE', #3001, #6435, #6475 ) ;
#4892 = VERTEX_POINT ( 'NONE', #1625 ) ;
#4893 = ORIENTED_EDGE ( 'NONE', *, *, #491, .F. ) ;
#4894 = ORIENTED_EDGE ( 'NONE', *, *, #7443, .F. ) ;
#4895 = DIRECTION ( 'NONE',  ( -0.000000000000000000, 1.000000000000000000, -0.000000000000000000 ) ) ;
#4896 = CARTESIAN_POINT ( 'NONE',  ( -4.211140560182196957, -2.431303136016552013, -3.745885042887436178 ) ) ;
#4897 = EDGE_CURVE ( 'NONE', #3177, #4028, #3540, .T. ) ;
#4898 = EDGE_LOOP ( 'NONE', ( #773, #2579, #4029, #2391 ) ) ;
#4899 = CARTESIAN_POINT ( 'NONE',  ( 0.000000000000000000, 0.000000000000000000, -4.974599999999998801 ) ) ;
#4900 = AXIS2_PLACEMENT_3D ( 'NONE', #3365, #6010, #4847 ) ;
#4901 = ORIENTED_EDGE ( 'NONE', *, *, #4330, .T. ) ;
#4902 = CARTESIAN_POINT ( 'NONE',  ( 0.000000000000000000, 0.000000000000000000, -4.000000000000000000 ) ) ;
#4903 = FACE_OUTER_BOUND ( 'NONE', #2158, .T. ) ;
#4904 = PLANE ( 'NONE',  #1272 ) ;
#4905 = ORIENTED_EDGE ( 'NONE', *, *, #3805, .F. ) ;
#4906 = AXIS2_PLACEMENT_3D ( 'NONE', #4557, #8578, #7876 ) ;
#4907 = EDGE_LOOP ( 'NONE', ( #3418, #4016, #4266, #3971 ) ) ;
#4908 = CARTESIAN_POINT ( 'NONE',  ( -5.000000000000000000, -5.000000000000000000, 140.0000000000000000 ) ) ;
#4909 = AXIS2_PLACEMENT_3D ( 'NONE', #151, #1431, #6867 ) ;
#4910 = CARTESIAN_POINT ( 'NONE',  ( 82.99999999999998579, 5.000000000000001776, 140.0000000000000000 ) ) ;
#4911 = AXIS2_PLACEMENT_3D ( 'NONE', #8222, #4776, #2081 ) ;
#4912 = CARTESIAN_POINT ( 'NONE',  ( 3.245314017740487441E-16, -25.00000000000000000, -160.1500000000000057 ) ) ;
#4913 = CARTESIAN_POINT ( 'NONE',  ( -0.02448733951239248641, -4.877042772274742255, -3.751161874094027571 ) ) ;
#4914 = ORIENTED_EDGE ( 'NONE', *, *, #551, .F. ) ;
#4915 = CIRCLE ( 'NONE', #37, 10.00000000000000000 ) ;
#4916 = STYLED_ITEM ( 'NONE', ( #1778 ), #3452 ) ;
#4917 = CARTESIAN_POINT ( 'NONE',  ( 2.500000000000000000, 2.357898499370433054, -1.951563910473907981E-15 ) ) ;
#4918 = ORIENTED_EDGE ( 'NONE', *, *, #7331, .T. ) ;
#4919 = ORIENTED_EDGE ( 'NONE', *, *, #3056, .F. ) ;
#4920 = EDGE_CURVE ( 'NONE', #2573, #7355, #285, .T. ) ;
#4921 = CARTESIAN_POINT ( 'NONE',  ( -2.712762565639006418, 3.052587955997511759, -3.430618716626627318 ) ) ;
#4922 = CARTESIAN_POINT ( 'NONE',  ( 20.00000000000000000, 140.0000000000000000, 5.000000000000000000 ) ) ;
#4923 = EDGE_CURVE ( 'NONE', #8570, #8480, #7450, .T. ) ;
#4924 = VECTOR ( 'NONE', #3854, 1000.000000000000000 ) ;
#4925 = ADVANCED_FACE ( 'NONE', ( #7590 ), #4320, .F. ) ;
#4926 = DIRECTION ( 'NONE',  ( 0.000000000000000000, 0.000000000000000000, -1.000000000000000000 ) ) ;
#4927 = CARTESIAN_POINT ( 'NONE',  ( 303.3333333333333144, -20.00000000000000000, 159.8500000000001080 ) ) ;
#4928 = EDGE_LOOP ( 'NONE', ( #3793, #8526, #4070, #2481 ) ) ;
#4929 = CARTESIAN_POINT ( 'NONE',  ( 82.99999999999998579, 5.000000000000001776, 139.9990000000000236 ) ) ;
#4930 = CIRCLE ( 'NONE', #6026, 10.00000000000000000 ) ;
#4931 = CARTESIAN_POINT ( 'NONE',  ( -2.344047193898593395, -3.265465875126480455, -1.054683074273691752E-14 ) ) ;
#4932 = CARTESIAN_POINT ( 'NONE',  ( -4.000000000000000000, 2.309401076758498483, -5.000000000000000000 ) ) ;
#4933 = CARTESIAN_POINT ( 'NONE',  ( -2.500000000000000444, 3.061616997868383634E-16, -25.03750572909317285 ) ) ;
#4934 = CARTESIAN_POINT ( 'NONE',  ( 181.0000000000000000, 5.000000000000000000, 139.9990000000000236 ) ) ;
#4935 = CARTESIAN_POINT ( 'NONE',  ( -5.000000000000001776, 5.000000000000001776, -0.9999999999999940048 ) ) ;
#4936 = EDGE_CURVE ( 'NONE', #7552, #4775, #5305, .T. ) ;
#4937 = ORIENTED_EDGE ( 'NONE', *, *, #1949, .F. ) ;
#4938 = ORIENTED_EDGE ( 'NONE', *, *, #8555, .F. ) ;
#4939 = ORIENTED_EDGE ( 'NONE', *, *, #2960, .F. ) ;
#4940 = ADVANCED_FACE ( 'NONE', ( #6184 ), #1672, .T. ) ;
#4941 = DIRECTION ( 'NONE',  ( -0.000000000000000000, 0.000000000000000000, 1.000000000000000000 ) ) ;
#4942 = LINE ( 'NONE', #366, #3809 ) ;
#4943 = ORIENTED_EDGE ( 'NONE', *, *, #7177, .F. ) ;
#4944 = AXIS2_PLACEMENT_3D ( 'NONE', #6445, #1883, #4520 ) ;
#4945 = DIRECTION ( 'NONE',  ( 0.000000000000000000, -1.000000000000000000, 0.000000000000000000 ) ) ;
#4946 = ORIENTED_EDGE ( 'NONE', *, *, #2311, .T. ) ;
#4947 =( LENGTH_UNIT ( ) NAMED_UNIT ( * ) SI_UNIT ( .MILLI., .METRE. ) );
#4948 = CARTESIAN_POINT ( 'NONE',  ( 269.0000000000000000, -4.999999999999998224, 140.0000000000000000 ) ) ;
#4949 = VERTEX_POINT ( 'NONE', #8121 ) ;
#4950 = UNCERTAINTY_MEASURE_WITH_UNIT (LENGTH_MEASURE( 1.000000000000000082E-05 ), #405, 'distance_accuracy_value', 'NONE');
#4951 = EDGE_LOOP ( 'NONE', ( #6644, #7444, #1365, #2991, #6672 ) ) ;
#4952 = FACE_OUTER_BOUND ( 'NONE', #5541, .T. ) ;
#4953 = CYLINDRICAL_SURFACE ( 'NONE', #2710, 20.00000000000000000 ) ;
#4954 = CIRCLE ( 'NONE', #6606, 5.384454397937118664 ) ;
#4955 = CIRCLE ( 'NONE', #3013, 2.041999999999999815 ) ;
#4956 = CARTESIAN_POINT ( 'NONE',  ( 0.000000000000000000, 0.000000000000000000, 5.000000000000000000 ) ) ;
#4957 = CARTESIAN_POINT ( 'NONE',  ( 53.33333333333330017, -25.00000000000000000, 162.5000000000000853 ) ) ;
#4958 = ORIENTED_EDGE ( 'NONE', *, *, #279, .F. ) ;
#4959 = AXIS2_PLACEMENT_3D ( 'NONE', #6190, #8211, #6365 ) ;
#4960 = AXIS2_PLACEMENT_3D ( 'NONE', #1103, #5225, #5058 ) ;
#4961 = DIRECTION ( 'NONE',  ( 1.000000000000000000, 1.734723475976807587E-16, 0.000000000000000000 ) ) ;
#4962 = ORIENTED_EDGE ( 'NONE', *, *, #2345, .T. ) ;
#4963 = ORIENTED_EDGE ( 'NONE', *, *, #5836, .T. ) ;
#4964 = CARTESIAN_POINT ( 'NONE',  ( -5.000000000000001776, 5.000000000000001776, -105.9999999999999858 ) ) ;
#4965 = FACE_BOUND ( 'NONE', #8349, .T. ) ;
#4966 = DIRECTION ( 'NONE',  ( -1.000000000000000000, 0.000000000000000000, 0.000000000000000000 ) ) ;
#4967 = DIRECTION ( 'NONE',  ( -0.000000000000000000, 1.000000000000000000, -0.000000000000000000 ) ) ;
#4968 = ORIENTED_EDGE ( 'NONE', *, *, #3025, .T. ) ;
#4969 = FACE_OUTER_BOUND ( 'NONE', #2073, .T. ) ;
#4970 = EDGE_CURVE ( 'NONE', #2803, #242, #8115, .T. ) ;
#4971 =( LENGTH_UNIT ( ) NAMED_UNIT ( * ) SI_UNIT ( .MILLI., .METRE. ) );
#4972 = ORIENTED_EDGE ( 'NONE', *, *, #3989, .F. ) ;
#4973 =( REPRESENTATION_RELATIONSHIP ('NONE','NONE', #3312, #872 ) REPRESENTATION_RELATIONSHIP_WITH_TRANSFORMATION ( #4463 )SHAPE_REPRESENTATION_RELATIONSHIP( ) );
#4974 = DIRECTION ( 'NONE',  ( 0.000000000000000000, -0.4999999999999993894, 0.8660254037844389297 ) ) ;
#4975 = EDGE_CURVE ( 'NONE', #3144, #874, #5864, .T. ) ;
#4976 = CARTESIAN_POINT ( 'NONE',  ( 0.000000000000000000, 0.000000000000000000, 120.0000000000000142 ) ) ;
#4977 = AXIS2_PLACEMENT_3D ( 'NONE', #7224, #7320, #1933 ) ;
#4978 = DIRECTION ( 'NONE',  ( -1.000000000000000000, -0.000000000000000000, -0.000000000000000000 ) ) ;
#4979 = CARTESIAN_POINT ( 'NONE',  ( -3.472371940586054251, -2.614027278893156669, -3.320322319202162031 ) ) ;
#4980 = VERTEX_POINT ( 'NONE', #3497 ) ;
#4981 = ORIENTED_EDGE ( 'NONE', *, *, #3732, .T. ) ;
#4982 = ORIENTED_EDGE ( 'NONE', *, *, #3167, .T. ) ;
#4983 = FACE_OUTER_BOUND ( 'NONE', #6957, .T. ) ;
#4984 = CARTESIAN_POINT ( 'NONE',  ( 0.000000000000000000, 0.000000000000000000, 0.000000000000000000 ) ) ;
#4985 = ORIENTED_EDGE ( 'NONE', *, *, #1731, .F. ) ;
#4986 = EDGE_LOOP ( 'NONE', ( #2856, #2395, #847, #1687 ) ) ;
#4987 = LINE ( 'NONE', #990, #7877 ) ;
#4988 = EDGE_LOOP ( 'NONE', ( #1568, #4644, #813, #5633 ) ) ;
#4989 = EDGE_LOOP ( 'NONE', ( #2368, #6082, #3346, #4914 ) ) ;
#4990 = FACE_OUTER_BOUND ( 'NONE', #8344, .T. ) ;
#4991 = AXIS2_PLACEMENT_3D ( 'NONE', #5274, #7943, #92 ) ;
#4992 = CARTESIAN_POINT ( 'NONE',  ( 303.3333333333333144, -20.00000000000000000, 159.8500000000001080 ) ) ;
#4993 = ADVANCED_FACE ( 'NONE', ( #8159 ), #6136, .T. ) ;
#4994 = EDGE_CURVE ( 'NONE', #3690, #6574, #164, .T. ) ;
#4995 = DIRECTION ( 'NONE',  ( 0.000000000000000000, 0.000000000000000000, -1.000000000000000000 ) ) ;
#4996 = VECTOR ( 'NONE', #446, 1000.000000000000000 ) ;
#4997 = CARTESIAN_POINT ( 'NONE',  ( 303.3333333333333144, -15.00000000000000000, 165.1500000000000625 ) ) ;
#4998 = ORIENTED_EDGE ( 'NONE', *, *, #5397, .T. ) ;
#4999 = DIRECTION ( 'NONE',  ( 1.000000000000000000, 9.912984321632765956E-19, 1.110223024625156540E-16 ) ) ;
#5000 = FACE_OUTER_BOUND ( 'NONE', #2241, .T. ) ;
#5001 = VERTEX_POINT ( 'NONE', #6842 ) ;
#5002 = VERTEX_POINT ( 'NONE', #886 ) ;
#5003 = DIRECTION ( 'NONE',  ( -0.000000000000000000, 1.000000000000000000, -0.000000000000000000 ) ) ;
#5004 = CARTESIAN_POINT ( 'NONE',  ( 264.0000000000000000, -20.00000000000000000, -48.78142504031547588 ) ) ;
#5005 = VECTOR ( 'NONE', #5449, 1000.000000000000000 ) ;
#5006 = PRODUCT_DEFINITION ( 'UNKNOWN', '', #3362, #5935 ) ;
#5007 = CARTESIAN_POINT ( 'NONE',  ( 5.000000000000000000, 5.000000000000000000, -0.9999999999999940048 ) ) ;
#5008 = DIRECTION ( 'NONE',  ( -0.000000000000000000, -0.000000000000000000, 1.000000000000000000 ) ) ;
#5009 = VERTEX_POINT ( 'NONE', #4884 ) ;
#5010 = DIRECTION ( 'NONE',  ( -0.000000000000000000, -0.000000000000000000, 1.000000000000000000 ) ) ;
#5011 = EDGE_LOOP ( 'NONE', ( #5996, #4943, #7715, #4475 ) ) ;
#5012 = PLANE ( 'NONE',  #2820 ) ;
#5013 = CARTESIAN_POINT ( 'NONE',  ( -5.000000000000000000, -5.000000000000000000, -143.0000000000000284 ) ) ;
#5014 = CYLINDRICAL_SURFACE ( 'NONE', #7091, 20.00000000000000000 ) ;
#5015 = CARTESIAN_POINT ( 'NONE',  ( 3.349226789952652439, 2.685125164760731487, -0.2236248678334773199 ) ) ;
#5016 = CARTESIAN_POINT ( 'NONE',  ( 0.000000000000000000, 0.000000000000000000, -4.484454397937119197 ) ) ;
#5017 = ORIENTED_EDGE ( 'NONE', *, *, #607, .F. ) ;
#5018 = AXIS2_PLACEMENT_3D ( 'NONE', #2359, #7046, #7753 ) ;
#5019 = ORIENTED_EDGE ( 'NONE', *, *, #2177, .T. ) ;
#5020 = CARTESIAN_POINT ( 'NONE',  ( 5.000000000000000000, 5.000000000000000000, -143.0000000000000284 ) ) ;
#5021 = DIRECTION ( 'NONE',  ( 0.000000000000000000, -1.000000000000000000, 0.000000000000000000 ) ) ;
#5022 = CIRCLE ( 'NONE', #1518, 20.00000000000000000 ) ;
#5023 = MECHANICAL_DESIGN_GEOMETRIC_PRESENTATION_REPRESENTATION (  '', ( #7816 ), #721 ) ;
#5024 = EDGE_CURVE ( 'NONE', #3247, #7213, #3238, .T. ) ;
#5025 = ORIENTED_EDGE ( 'NONE', *, *, #8072, .T. ) ;
#5026 =( NAMED_UNIT ( * ) PLANE_ANGLE_UNIT ( ) SI_UNIT ( $, .RADIAN. ) );
#5027 = ORIENTED_EDGE ( 'NONE', *, *, #841, .F. ) ;
#5028 =( NAMED_UNIT ( * ) PLANE_ANGLE_UNIT ( ) SI_UNIT ( $, .RADIAN. ) );
#5029 = CARTESIAN_POINT ( 'NONE',  ( 4.197393957002303999, 7.772902908466098641E-14, -3.503767560748929810 ) ) ;
#5030 = EDGE_LOOP ( 'NONE', ( #3901, #208, #117, #1127 ) ) ;
#5031 = VERTEX_POINT ( 'NONE', #3582 ) ;
#5032 = DIRECTION ( 'NONE',  ( 0.000000000000000000, 0.000000000000000000, -1.000000000000000000 ) ) ;
#5033 = AXIS2_PLACEMENT_3D ( 'NONE', #7211, #2527, #3216 ) ;
#5034 = DIRECTION ( 'NONE',  ( -1.000000000000000000, 1.734723475976807587E-16, 0.000000000000000000 ) ) ;
#5035 =( BOUNDED_SURFACE ( )  B_SPLINE_SURFACE ( 3, 2, ( 
 ( #225, #1676, #2337 ),
 ( #4979, #3676, #7596 ),
 ( #4238, #6276, #2380 ),
 ( #8165, #6799, #2198 ),
 ( #181, #2848, #7503 ),
 ( #8298, #5496, #315 ) ),
 .UNSPECIFIED., .F., .F., .F. ) 
 B_SPLINE_SURFACE_WITH_KNOTS ( ( 4, 2, 4 ),
 ( 3, 3 ),
 ( 0.02032853247518126918, 0.02278863295364821906, 0.02524873343211516893 ),
 ( 0.000000000000000000, 1.000000000000000000 ),
 .UNSPECIFIED. ) 
 GEOMETRIC_REPRESENTATION_ITEM ( )  RATIONAL_B_SPLINE_SURFACE ( (
 ( 1.000000000000000000, 0.8047781615896838492, 1.000000000000000000),
 ( 1.000000000000000000, 0.8123767586288186404, 1.000000000000000000),
 ( 1.000000000000000000, 0.8190662415565814758, 1.000000000000000000),
 ( 1.000000000000000000, 0.8192361015667604107, 1.000000000000000000),
 ( 1.000000000000000000, 0.8126135807104967190, 1.000000000000000000),
 ( 1.000000000000000000, 0.8047712338318580017, 1.000000000000000000) ) ) 
 REPRESENTATION_ITEM ( '' )  SURFACE ( )  );
#5036 = CIRCLE ( 'NONE', #308, 20.00000000000000000 ) ;
#5037 = CARTESIAN_POINT ( 'NONE',  ( 5.000000000000002665, 3.306546357697854226E-16, 2.700000000000001066 ) ) ;
#5038 = CARTESIAN_POINT ( 'NONE',  ( -3.333333333333332149, -2.694301256218264218, -3.300726591567082036 ) ) ;
#5039 = ORIENTED_EDGE ( 'NONE', *, *, #7605, .T. ) ;
#5040 = VECTOR ( 'NONE', #8422, 1000.000000000000000 ) ;
#5041 = EDGE_CURVE ( 'NONE', #1514, #771, #6229, .T. ) ;
#5042 = CARTESIAN_POINT ( 'NONE',  ( 352.0000000000000000, -20.00000000000000355, 141.2685749596845710 ) ) ;
#5043 = PLANE ( 'NONE',  #3756 ) ;
#5044 = ORIENTED_EDGE ( 'NONE', *, *, #2865, .F. ) ;
#5045 = VERTEX_POINT ( 'NONE', #5572 ) ;
#5046 = VECTOR ( 'NONE', #5938, 1000.000000000000000 ) ;
#5047 = CARTESIAN_POINT ( 'NONE',  ( 53.33333333333330017, -14.99999999999999822, 162.5000000000000853 ) ) ;
#5048 = DIRECTION ( 'NONE',  ( -0.000000000000000000, -0.000000000000000000, 1.000000000000000000 ) ) ;
#5049 = AXIS2_PLACEMENT_3D ( 'NONE', #7758, #5003, #1795 ) ;
#5050 = COLOUR_RGB ( '',0.8941176470588234615, 0.8941176470588234615, 0.8941176470588234615 ) ;
#5051 = CARTESIAN_POINT ( 'NONE',  ( 0.000000000000000000, 0.000000000000000000, 0.000000000000000000 ) ) ;
#5052 = CARTESIAN_POINT ( 'NONE',  ( -31.74999999999995737, 0.000000000000000000, 0.000000000000000000 ) ) ;
#5053 = VERTEX_POINT ( 'NONE', #5621 ) ;
#5054 = ORIENTED_EDGE ( 'NONE', *, *, #4298, .F. ) ;
#5055 = DIRECTION ( 'NONE',  ( 0.000000000000000000, 0.000000000000000000, -1.000000000000000000 ) ) ;
#5056 = TOROIDAL_SURFACE ( 'NONE', #475, 2.700000000000001066, 0.2000000000000000111 ) ;
#5057 = CARTESIAN_POINT ( 'NONE',  ( 136.6666666666666288, -20.00000000000000000, 159.8500000000001080 ) ) ;
#5058 = DIRECTION ( 'NONE',  ( 1.000000000000000000, 0.000000000000000000, -0.000000000000000000 ) ) ;
#5059 = CARTESIAN_POINT ( 'NONE',  ( 136.6666666666666288, -15.00000000000000000, 165.1500000000000625 ) ) ;
#5060 = DIRECTION ( 'NONE',  ( 0.000000000000000000, 0.000000000000000000, 1.000000000000000000 ) ) ;
#5061 = VECTOR ( 'NONE', #4353, 1000.000000000000000 ) ;
#5062 = EDGE_LOOP ( 'NONE', ( #7710, #4562, #4901, #386 ) ) ;
#5063 = CARTESIAN_POINT ( 'NONE',  ( 5.000000000000000000, -5.000000000000000000, -36.00000000000000000 ) ) ;
#5064 = CARTESIAN_POINT ( 'NONE',  ( -6.259644161404860030E-16, -4.618802153517027165, -3.433295621305388234 ) ) ;
#5065 = CARTESIAN_POINT ( 'NONE',  ( -20.00000000000000000, 2.449293598294706513E-15, -43.99999999999997158 ) ) ;
#5066 = UNCERTAINTY_MEASURE_WITH_UNIT (LENGTH_MEASURE( 1.000000000000000082E-05 ), #5349, 'distance_accuracy_value', 'NONE');
#5067 = ORIENTED_EDGE ( 'NONE', *, *, #1654, .F. ) ;
#5068 = DIRECTION ( 'NONE',  ( 0.000000000000000000, 0.000000000000000000, 1.000000000000000000 ) ) ;
#5069 = ADVANCED_FACE ( 'NONE', ( #5704, #2462 ), #5791, .T. ) ;
#5070 = VERTEX_POINT ( 'NONE', #352 ) ;
#5071 = DIRECTION ( 'NONE',  ( 0.000000000000000000, 0.000000000000000000, 1.000000000000000000 ) ) ;
#5072 = CARTESIAN_POINT ( 'NONE',  ( 219.9999999999999716, -20.00000000000000000, 165.1500000000000625 ) ) ;
#5073 = ADVANCED_FACE ( 'NONE', ( #3752 ), #8501, .F. ) ;
#5074 = ITEM_DEFINED_TRANSFORMATION ( 'NONE', 'NONE', #148,  #594 ) ;
#5075 = VERTEX_POINT ( 'NONE', #1057 ) ;
#5076 = ORIENTED_EDGE ( 'NONE', *, *, #8521, .T. ) ;
#5077 = CARTESIAN_POINT ( 'NONE',  ( 347.0000000000000000, 5.000000000000001776, 139.9990000000000236 ) ) ;
#5078 = EDGE_CURVE ( 'NONE', #4892, #3700, #8464, .T. ) ;
#5079 = DIRECTION ( 'NONE',  ( -0.000000000000000000, -0.000000000000000000, -1.000000000000000000 ) ) ;
#5080 = VECTOR ( 'NONE', #3648, 1000.000000000000000 ) ;
#5081 = CARTESIAN_POINT ( 'NONE',  ( 136.6666666666666288, -20.00000000000000000, 162.5000000000000853 ) ) ;
#5082 = VERTEX_POINT ( 'NONE', #6317 ) ;
#5083 = CARTESIAN_POINT ( 'NONE',  ( 264.0000000000000000, 0.000000000000000000, 0.000000000000000000 ) ) ;
#5084 = DIRECTION ( 'NONE',  ( 1.000000000000000000, 0.000000000000000000, 0.000000000000000000 ) ) ;
#5085 = EDGE_LOOP ( 'NONE', ( #5802, #3434 ) ) ;
#5086 = ORIENTED_EDGE ( 'NONE', *, *, #4807, .T. ) ;
#5087 = VECTOR ( 'NONE', #2040, 1000.000000000000000 ) ;
#5088 = CARTESIAN_POINT ( 'NONE',  ( -5.000000000000000000, -5.000000000000000000, 148.0000000000000284 ) ) ;
#5089 = CARTESIAN_POINT ( 'NONE',  ( -5.000000000000001776, 5.000000000000001776, 148.0000000000000284 ) ) ;
#5090 = CIRCLE ( 'NONE', #6897, 2.500000000000000444 ) ;
#5091 = CARTESIAN_POINT ( 'NONE',  ( 136.6666666666666288, -15.00000000000000000, 162.5000000000000853 ) ) ;
#5092 = AXIS2_PLACEMENT_3D ( 'NONE', #2902, #8311, #6987 ) ;
#5093 = PLANE ( 'NONE',  #4289 ) ;
#5094 = ORIENTED_EDGE ( 'NONE', *, *, #6239, .F. ) ;
#5095 = ORIENTED_EDGE ( 'NONE', *, *, #4278, .T. ) ;
#5096 = DIRECTION ( 'NONE',  ( -1.000000000000000000, 0.000000000000000000, 0.000000000000000000 ) ) ;
#5097 = MECHANICAL_DESIGN_GEOMETRIC_PRESENTATION_REPRESENTATION (  '', ( #651 ), #6904 ) ;
#5098 = AXIS2_PLACEMENT_3D ( 'NONE', #1760, #1144, #3151 ) ;
#5099 = ADVANCED_FACE ( 'NONE', ( #3018 ), #5012, .T. ) ;
#5100 = ADVANCED_FACE ( 'NONE', ( #4487 ), #3063, .F. ) ;
#5101 = DIRECTION ( 'NONE',  ( 0.000000000000000000, -1.000000000000000000, 0.000000000000000000 ) ) ;
#5102 = DIRECTION ( 'NONE',  ( -0.000000000000000000, -0.000000000000000000, -1.000000000000000000 ) ) ;
#5103 = EDGE_CURVE ( 'NONE', #5212, #3427, #4448, .T. ) ;
#5104 = CYLINDRICAL_SURFACE ( 'NONE', #546, 10.00000000000000000 ) ;
#5105 = CARTESIAN_POINT ( 'NONE',  ( -2.649999999999987477, 157.5000000000000284, 5.000000000000000888 ) ) ;
#5106 = ORIENTED_EDGE ( 'NONE', *, *, #914, .T. ) ;
#5107 = FILL_AREA_STYLE ('',( #1647 ) ) ;
#5108 = CARTESIAN_POINT ( 'NONE',  ( 0.000000000000000000, 0.000000000000000000, -135.0000000000000000 ) ) ;
#5109 = VECTOR ( 'NONE', #2831, 1000.000000000000000 ) ;
#5110 = CARTESIAN_POINT ( 'NONE',  ( 470.0000000000000000, 15.00000000000000000, 145.0000000000000284 ) ) ;
#5111 = PRODUCT_DEFINITION_SHAPE ( 'NONE', 'NONE',  #8620 ) ;
#5112 = ADVANCED_FACE ( 'NONE', ( #7098 ), #6808, .F. ) ;
#5113 = B_SPLINE_CURVE_WITH_KNOTS ( 'NONE', 3,
 ( #774, #2164, #5419, #3428, #7514, #8180, #102, #2208 ),
 .UNSPECIFIED., .F., .F.,
 ( 4, 2, 2, 4 ),
 ( 0.000000000000000000, 0.002450665683189819262, 0.003675998524784728893, 0.004901331366379639391 ),
 .UNSPECIFIED. ) ;
#5114 = ORIENTED_EDGE ( 'NONE', *, *, #5888, .T. ) ;
#5115 = LINE ( 'NONE', #6463, #7316 ) ;
#5116 = ORIENTED_EDGE ( 'NONE', *, *, #4923, .F. ) ;
#5117 = SURFACE_STYLE_FILL_AREA ( #7160 ) ;
#5118 = PLANE ( 'NONE',  #7182 ) ;
#5119 = ORIENTED_EDGE ( 'NONE', *, *, #7096, .F. ) ;
#5120 = ORIENTED_EDGE ( 'NONE', *, *, #7799, .T. ) ;
#5121 = CARTESIAN_POINT ( 'NONE',  ( -4.204015924366189871, 1.626724848190922446, -3.610627190413390419 ) ) ;
#5122 = DIRECTION ( 'NONE',  ( -0.000000000000000000, -0.000000000000000000, -1.000000000000000000 ) ) ;
#5123 = VECTOR ( 'NONE', #6650, 1000.000000000000000 ) ;
#5124 = CARTESIAN_POINT ( 'NONE',  ( -5.000000000000001776, 5.000000000000001776, 34.00000000000000711 ) ) ;
#5125 = ORIENTED_EDGE ( 'NONE', *, *, #120, .F. ) ;
#5126 = EDGE_CURVE ( 'NONE', #4010, #5500, #8334, .T. ) ;
#5127 = VECTOR ( 'NONE', #4627, 1000.000000000000000 ) ;
#5128 = CARTESIAN_POINT ( 'NONE',  ( 303.3333333333333144, -30.00000000000000355, 162.5000000000000853 ) ) ;
#5129 = FACE_OUTER_BOUND ( 'NONE', #6817, .T. ) ;
#5130 = ORIENTED_EDGE ( 'NONE', *, *, #6116, .T. ) ;
#5131 = ORIENTED_EDGE ( 'NONE', *, *, #120, .T. ) ;
#5132 = DIRECTION ( 'NONE',  ( -0.000000000000000000, 1.000000000000000000, -0.000000000000000000 ) ) ;
#5133 = CARTESIAN_POINT ( 'NONE',  ( -30.00000000000002842, -25.00000000000000000, 200.0000000000000000 ) ) ;
#5134 = AXIS2_PLACEMENT_3D ( 'NONE', #6533, #4452, #7152 ) ;
#5135 = EDGE_CURVE ( 'NONE', #7063, #6851, #1277, .T. ) ;
#5136 = CARTESIAN_POINT ( 'NONE',  ( 5.000000000000001776, 134.9989999999999952, 15.00000000000000355 ) ) ;
#5137 = CYLINDRICAL_SURFACE ( 'NONE', #6230, 2.649999999999985700 ) ;
#5138 = EDGE_LOOP ( 'NONE', ( #4545, #3781, #2099, #1831 ) ) ;
#5139 = ADVANCED_FACE ( 'NONE', ( #3797 ), #4525, .F. ) ;
#5140 = ORIENTED_EDGE ( 'NONE', *, *, #7440, .T. ) ;
#5141 = VERTEX_POINT ( 'NONE', #1717 ) ;
#5142 = AXIS2_PLACEMENT_3D ( 'NONE', #3328, #2026, #5968 ) ;
#5143 = CARTESIAN_POINT ( 'NONE',  ( 0.000000000000000000, 0.000000000000000000, -77.99999999999997158 ) ) ;
#5144 = CARTESIAN_POINT ( 'NONE',  ( -0.6507732100473471171, 4.243078065514775510, -0.2236248678334823436 ) ) ;
#5145 = AXIS2_PLACEMENT_3D ( 'NONE', #3002, #7620, #5609 ) ;
#5146 = CYLINDRICAL_SURFACE ( 'NONE', #4031, 10.00000000000000000 ) ;
#5147 = CARTESIAN_POINT ( 'NONE',  ( 2.500000000000000000, -2.357898499370432610, 3.252606517456513302E-15 ) ) ;
#5148 = SURFACE_SIDE_STYLE ('',( #3890 ) ) ;
#5149 = EDGE_CURVE ( 'NONE', #7186, #2677, #5826, .T. ) ;
#5150 = FACE_OUTER_BOUND ( 'NONE', #7460, .T. ) ;
#5151 = LINE ( 'NONE', #5964, #4366 ) ;
#5152 = LINE ( 'NONE', #4623, #2544 ) ;
#5153 = CARTESIAN_POINT ( 'NONE',  ( 25.00000000000000000, 0.000000000000000000, 0.000000000000000000 ) ) ;
#5154 = ORIENTED_EDGE ( 'NONE', *, *, #981, .F. ) ;
#5155 =( NAMED_UNIT ( * ) PLANE_ANGLE_UNIT ( ) SI_UNIT ( $, .RADIAN. ) );
#5156 = CARTESIAN_POINT ( 'NONE',  ( 10.00000000000000000, 0.000000000000000000, -135.0000000000000000 ) ) ;
#5157 = ORIENTED_EDGE ( 'NONE', *, *, #681, .T. ) ;
#5158 = CARTESIAN_POINT ( 'NONE',  ( 0.6666666666666689611, 4.233901974057261874, -3.300726591567082480 ) ) ;
#5159 = CARTESIAN_POINT ( 'NONE',  ( 1.144235203016666258, 3.958177651039090250, -0.09382832055445661235 ) ) ;
#5160 = MECHANICAL_DESIGN_GEOMETRIC_PRESENTATION_REPRESENTATION (  '', ( #3777 ), #2536 ) ;
#5161 = EDGE_CURVE ( 'NONE', #8500, #5001, #6698, .T. ) ;
#5162 = DIRECTION ( 'NONE',  ( 0.000000000000000000, 1.000000000000000000, 0.000000000000000000 ) ) ;
#5163 = ORIENTED_EDGE ( 'NONE', *, *, #5888, .F. ) ;
#5164 = CYLINDRICAL_SURFACE ( 'NONE', #6147, 20.00000000000000000 ) ;
#5165 = AXIS2_PLACEMENT_3D ( 'NONE', #1701, #2526, #1658 ) ;
#5166 = CARTESIAN_POINT ( 'NONE',  ( 53.33333333333332860, -29.99999999999999645, 162.5000000000001705 ) ) ;
#5167 = DIRECTION ( 'NONE',  ( -0.000000000000000000, -0.000000000000000000, 1.000000000000000000 ) ) ;
#5168 = ORIENTED_EDGE ( 'NONE', *, *, #4173, .T. ) ;
#5169 = AXIS2_PLACEMENT_3D ( 'NONE', #1555, #2045, #4123 ) ;
#5170 = ORIENTED_EDGE ( 'NONE', *, *, #3300, .T. ) ;
#5171 = CARTESIAN_POINT ( 'NONE',  ( -5.000000000000000000, -5.000000000000000000, 34.00000000000000711 ) ) ;
#5172 = CARTESIAN_POINT ( 'NONE',  ( 0.000000000000000000, 0.000000000000000000, -120.5685424949237898 ) ) ;
#5173 = DIRECTION ( 'NONE',  ( 0.000000000000000000, 0.000000000000000000, 1.000000000000000000 ) ) ;
#5174 = DIRECTION ( 'NONE',  ( 0.000000000000000000, 0.000000000000000000, -1.000000000000000000 ) ) ;
#5175 = ORIENTED_EDGE ( 'NONE', *, *, #3538, .F. ) ;
#5176 = EDGE_CURVE ( 'NONE', #5424, #1367, #3924, .T. ) ;
#5177 = VECTOR ( 'NONE', #7870, 1000.000000000000000 ) ;
#5178 = EDGE_CURVE ( 'NONE', #8421, #8315, #5872, .T. ) ;
#5179 = SHAPE_REPRESENTATION_RELATIONSHIP ( 'NONE' , 'NONE' ,  #872, #1476 ) ;
#5180 = ORIENTED_EDGE ( 'NONE', *, *, #7283, .T. ) ;
#5181 = EDGE_CURVE ( 'NONE', #4379, #1747, #6569, .T. ) ;
#5182 = AXIS2_PLACEMENT_3D ( 'NONE', #6083, #2963, #5612 ) ;
#5183 = EDGE_CURVE ( 'NONE', #3913, #8141, #7123, .T. ) ;
#5184 = AXIS2_PLACEMENT_3D ( 'NONE', #7378, #2807, #854 ) ;
#5185 = STYLED_ITEM ( 'NONE', ( #394 ), #1476 ) ;
#5186 = PLANE ( 'NONE',  #4960 ) ;
#5187 = DIRECTION ( 'NONE',  ( -0.000000000000000000, -0.000000000000000000, 1.000000000000000000 ) ) ;
#5188 = DIRECTION ( 'NONE',  ( -0.000000000000000000, -0.000000000000000000, -1.000000000000000000 ) ) ;
#5189 = SURFACE_STYLE_FILL_AREA ( #7891 ) ;
#5190 = AXIS2_PLACEMENT_3D ( 'NONE', #1977, #4622, #1317 ) ;
#5191 = SURFACE_STYLE_USAGE ( .BOTH. , #5799 ) ;
#5192 = DIRECTION ( 'NONE',  ( -0.000000000000000000, 1.000000000000000000, -0.000000000000000000 ) ) ;
#5193 = CARTESIAN_POINT ( 'NONE',  ( 4.000000000000000000, -2.309401076758514915, -3.433295621305383349 ) ) ;
#5194 = VECTOR ( 'NONE', #212, 1000.000000000000000 ) ;
#5195 = EDGE_CURVE ( 'NONE', #1599, #4765, #3356, .T. ) ;
#5196 = DIRECTION ( 'NONE',  ( 0.000000000000000000, 0.000000000000000000, 1.000000000000000000 ) ) ;
#5197 = LINE ( 'NONE', #4628, #3851 ) ;
#5198 = ORIENTED_EDGE ( 'NONE', *, *, #4936, .F. ) ;
#5199 =( LENGTH_UNIT ( ) NAMED_UNIT ( * ) SI_UNIT ( .MILLI., .METRE. ) );
#5200 = CARTESIAN_POINT ( 'NONE',  ( -5.000000000000000000, -5.000000000000000000, -36.00000000000000000 ) ) ;
#5201 = ORIENTED_EDGE ( 'NONE', *, *, #7205, .F. ) ;
#5202 = CARTESIAN_POINT ( 'NONE',  ( 10.00000000000000000, 0.000000000000000000, 140.0000000000000000 ) ) ;
#5203 = DIRECTION ( 'NONE',  ( 1.734723475976806848E-16, -1.000000000000000000, -0.000000000000000000 ) ) ;
#5204 = EDGE_CURVE ( 'NONE', #808, #848, #2751, .T. ) ;
#5205 = DIRECTION ( 'NONE',  ( 0.000000000000000000, 0.000000000000000000, 1.000000000000000000 ) ) ;
#5206 = EDGE_LOOP ( 'NONE', ( #8184, #5627, #1297, #1838 ) ) ;
#5207 = DIRECTION ( 'NONE',  ( -0.000000000000000000, -0.000000000000000000, 1.000000000000000000 ) ) ;
#5208 = ADVANCED_FACE ( 'NONE', ( #8588 ), #6696, .F. ) ;
#5209 = DIRECTION ( 'NONE',  ( -2.081668171172168513E-17, -1.000000000000000000, 1.110223024625156540E-16 ) ) ;
#5210 = FACE_BOUND ( 'NONE', #2840, .T. ) ;
#5211 = ORIENTED_EDGE ( 'NONE', *, *, #8262, .T. ) ;
#5212 = VERTEX_POINT ( 'NONE', #5910 ) ;
#5213 = DIRECTION ( 'NONE',  ( -1.000000000000000000, 1.734723475976806848E-16, -0.000000000000000000 ) ) ;
#5214 = CARTESIAN_POINT ( 'NONE',  ( 5.000000000000000000, -5.000000000000000000, -63.99999999999997158 ) ) ;
#5215 = DIRECTION ( 'NONE',  ( -1.000000000000000000, -0.000000000000000000, -0.000000000000000000 ) ) ;
#5216 = DIRECTION ( 'NONE',  ( 0.000000000000000000, 0.000000000000000000, 1.000000000000000000 ) ) ;
#5217 = ORIENTED_EDGE ( 'NONE', *, *, #1141, .F. ) ;
#5218 = AXIS2_PLACEMENT_3D ( 'NONE', #5051, #6354, #4356 ) ;
#5219 = PRESENTATION_STYLE_ASSIGNMENT (( #613 ) ) ;
#5220 = EDGE_LOOP ( 'NONE', ( #6549, #1984 ) ) ;
#5221 = DIRECTION ( 'NONE',  ( 0.000000000000000000, 0.000000000000000000, 1.000000000000000000 ) ) ;
#5222 = EDGE_CURVE ( 'NONE', #1611, #3710, #8527, .T. ) ;
#5223 = AXIS2_PLACEMENT_3D ( 'NONE', #5081, #5808, #8484 ) ;
#5224 = CLOSED_SHELL ( 'NONE', ( #1758, #1623, #8236, #2792, #8170, #3844, #6269, #2711, #5328, #1116, #2101, #2933, #8199, #5709, #2061, #2153, #8568, #7109, #1800, #1017, #6156, #8335, #4725, #3350, #2975, #2194, #1122, #5297, #5112, #3906, #748, #2808 ) ) ;
#5225 = DIRECTION ( 'NONE',  ( 0.000000000000000000, 0.000000000000000000, 1.000000000000000000 ) ) ;
#5226 = CARTESIAN_POINT ( 'NONE',  ( -10.00000000000000000, 1.224646799147353256E-15, 7.000000000000006217 ) ) ;
#5227 = CARTESIAN_POINT ( 'NONE',  ( 136.6666666666666288, -14.99999999999999822, 165.1500000000000625 ) ) ;
#5228 = EDGE_CURVE ( 'NONE', #8533, #8315, #4701, .T. ) ;
#5229 = CIRCLE ( 'NONE', #4959, 2.649999999999985700 ) ;
#5230 = AXIS2_PLACEMENT_3D ( 'NONE', #8288, #3533, #1666 ) ;
#5231 = CARTESIAN_POINT ( 'NONE',  ( 2.000000000000008882, 3.464101615137749945, 0.000000000000000000 ) ) ;
#5232 = CARTESIAN_POINT ( 'NONE',  ( 470.0000000000000000, -15.00000000000000000, 145.0000000000000284 ) ) ;
#5233 = CARTESIAN_POINT ( 'NONE',  ( 4.000000000000000000, 0.7924765000094659007, -0.05906175389889852662 ) ) ;
#5234 = DIRECTION ( 'NONE',  ( -0.000000000000000000, 0.000000000000000000, -1.000000000000000000 ) ) ;
#5235 = DIRECTION ( 'NONE',  ( 0.000000000000000000, 0.000000000000000000, 1.000000000000000000 ) ) ;
#5236 = SURFACE_STYLE_FILL_AREA ( #8557 ) ;
#5237 = VERTEX_POINT ( 'NONE', #6042 ) ;
#5238 = FACE_OUTER_BOUND ( 'NONE', #2580, .T. ) ;
#5239 = ORIENTED_EDGE ( 'NONE', *, *, #5443, .F. ) ;
#5240 = APPLICATION_CONTEXT ( 'automotive_design' ) ;
#5241 = FACE_OUTER_BOUND ( 'NONE', #6600, .T. ) ;
#5242 = DIRECTION ( 'NONE',  ( 1.000000000000000000, 0.000000000000000000, -0.000000000000000000 ) ) ;
#5243 = PRODUCT_DEFINITION_CONTEXT ( 'detailed design', #4186, 'design' ) ;
#5244 = CARTESIAN_POINT ( 'NONE',  ( 82.99999999999998579, 5.000000000000001776, 140.0000000000000000 ) ) ;
#5245 = ORIENTED_EDGE ( 'NONE', *, *, #2946, .T. ) ;
#5246 = CARTESIAN_POINT ( 'NONE',  ( 0.000000000000000000, -20.00000000000000000, -154.8500000000000512 ) ) ;
#5247 = CARTESIAN_POINT ( 'NONE',  ( -5.000000000000000000, -5.000000000000000000, -36.00000000000000000 ) ) ;
#5248 = EDGE_LOOP ( 'NONE', ( #2915, #8010, #1715, #5175 ) ) ;
#5249 = ORIENTED_EDGE ( 'NONE', *, *, #5547, .F. ) ;
#5250 = EDGE_CURVE ( 'NONE', #2610, #8019, #36, .T. ) ;
#5251 = DIRECTION ( 'NONE',  ( -1.000000000000000000, 1.734723475976806848E-16, -0.000000000000000000 ) ) ;
#5252 = AXIS2_PLACEMENT_3D ( 'NONE', #3968, #610, #1257 ) ;
#5253 = ADVANCED_FACE ( 'NONE', ( #7886 ), #2095, .F. ) ;
#5254 = DIRECTION ( 'NONE',  ( 0.000000000000000000, 0.000000000000000000, -1.000000000000000000 ) ) ;
#5255 = CARTESIAN_POINT ( 'NONE',  ( 10.00000000000000000, 0.000000000000000000, 42.00000000000000711 ) ) ;
#5256 = CIRCLE ( 'NONE', #4569, 0.5155456020628804703 ) ;
#5257 = DIRECTION ( 'NONE',  ( 0.000000000000000000, 0.000000000000000000, -1.000000000000000000 ) ) ;
#5258 = ORIENTED_EDGE ( 'NONE', *, *, #6651, .T. ) ;
#5259 = VERTEX_POINT ( 'NONE', #6528 ) ;
#5260 = DIRECTION ( 'NONE',  ( 0.000000000000000000, 1.000000000000000000, 0.000000000000000000 ) ) ;
#5261 = AXIS2_PLACEMENT_3D ( 'NONE', #3, #2676, #4067 ) ;
#5262 = EDGE_CURVE ( 'NONE', #7313, #6803, #4074, .T. ) ;
#5263 = DIRECTION ( 'NONE',  ( 0.000000000000000000, 0.000000000000000000, 1.000000000000000000 ) ) ;
#5264 = DIRECTION ( 'NONE',  ( -1.000000000000000000, 0.000000000000000000, -0.000000000000000000 ) ) ;
#5265 = VERTEX_POINT ( 'NONE', #2619 ) ;
#5266 = LINE ( 'NONE', #3930, #7216 ) ;
#5267 = DIRECTION ( 'NONE',  ( 1.000000000000000000, 0.000000000000000000, 0.000000000000000000 ) ) ;
#5268 = CIRCLE ( 'NONE', #2777, 2.649999999999985700 ) ;
#5269 = CARTESIAN_POINT ( 'NONE',  ( -5.000000000000001776, 5.000000000000001776, 42.00000000000000711 ) ) ;
#5270 = FACE_OUTER_BOUND ( 'NONE', #5348, .T. ) ;
#5271 = CARTESIAN_POINT ( 'NONE',  ( 0.2500000000000002220, 0.000000000000000000, 0.000000000000000000 ) ) ;
#5272 = VECTOR ( 'NONE', #7768, 1000.000000000000000 ) ;
#5273 = DIRECTION ( 'NONE',  ( 0.000000000000000000, 0.000000000000000000, 1.000000000000000000 ) ) ;
#5274 = CARTESIAN_POINT ( 'NONE',  ( 0.000000000000000000, 0.000000000000000000, 120.0000000000000142 ) ) ;
#5275 = DIRECTION ( 'NONE',  ( -1.000000000000000000, -0.000000000000000000, -0.000000000000000000 ) ) ;
#5276 = ORIENTED_EDGE ( 'NONE', *, *, #4920, .F. ) ;
#5277 = PRESENTATION_STYLE_ASSIGNMENT (( #1238 ) ) ;
#5278 = EDGE_LOOP ( 'NONE', ( #1336, #4454 ) ) ;
#5279 = EDGE_CURVE ( 'NONE', #5393, #1782, #4488, .T. ) ;
#5280 = ORIENTED_EDGE ( 'NONE', *, *, #1456, .T. ) ;
#5281 = CARTESIAN_POINT ( 'NONE',  ( 5.000000000000000000, 5.000000000000000000, 148.0000000000000284 ) ) ;
#5282 = EDGE_CURVE ( 'NONE', #3371, #1280, #566, .T. ) ;
#5283 = DIRECTION ( 'NONE',  ( 0.000000000000000000, 1.000000000000000000, 0.000000000000000000 ) ) ;
#5284 = EDGE_CURVE ( 'NONE', #1556, #3270, #7222, .T. ) ;
#5285 = CARTESIAN_POINT ( 'NONE',  ( 2.499999999999999556, 0.000000000000000000, 3.469446951953614189E-15 ) ) ;
#5286 = VERTEX_POINT ( 'NONE', #5304 ) ;
#5287 = CARTESIAN_POINT ( 'NONE',  ( 219.9999999999999716, -20.00000000000000000, 159.8500000000001080 ) ) ;
#5288 = DIRECTION ( 'NONE',  ( -1.000000000000000000, 1.734723475976807587E-16, 0.000000000000000000 ) ) ;
#5289 = DIRECTION ( 'NONE',  ( 1.994931997373328159E-17, -1.000000000000000000, -1.110223024625156540E-16 ) ) ;
#5290 = FACE_OUTER_BOUND ( 'NONE', #4420, .T. ) ;
#5291 = ORIENTED_EDGE ( 'NONE', *, *, #6565, .T. ) ;
#5292 = ORIENTED_EDGE ( 'NONE', *, *, #4612, .T. ) ;
#5293 = PRESENTATION_LAYER_ASSIGNMENT (  '', '', ( #6410 ) ) ;
#5294 = LINE ( 'NONE', #1218, #2277 ) ;
#5295 = LINE ( 'NONE', #5214, #1448 ) ;
#5296 = CARTESIAN_POINT ( 'NONE',  ( 4.197478902586992966, -0.8524102783748346290, -3.505063281295504041 ) ) ;
#5297 = ADVANCED_FACE ( 'NONE', ( #2014 ), #6200, .F. ) ;
#5298 = AXIS2_PLACEMENT_3D ( 'NONE', #5083, #3828, #8489 ) ;
#5299 = PRODUCT_DEFINITION_SHAPE ( 'NONE', 'NONE',  #2571 ) ;
#5300 = DIRECTION ( 'NONE',  ( 1.000000000000000000, 0.000000000000000000, 0.000000000000000000 ) ) ;
#5301 = ORIENTED_EDGE ( 'NONE', *, *, #6187, .F. ) ;
#5302=STYLED_ITEM('',(#8678),#4757);
#5303 = ORIENTED_EDGE ( 'NONE', *, *, #5041, .T. ) ;
#5304 = CARTESIAN_POINT ( 'NONE',  ( 357.0000000000000000, -4.999999999999998224, 145.0000000000000284 ) ) ;
#5305 = CIRCLE ( 'NONE', #6287, 4.000000000000000000 ) ;
#5306 = VECTOR ( 'NONE', #3583, 1000.000000000000000 ) ;
#5307 = DIRECTION ( 'NONE',  ( 0.000000000000000000, 0.000000000000000000, -1.000000000000000000 ) ) ;
#5308 = CARTESIAN_POINT ( 'NONE',  ( 0.000000000000000000, 0.000000000000000000, -7.999999999999992895 ) ) ;
#5309 = ORIENTED_EDGE ( 'NONE', *, *, #3808, .T. ) ;
#5310 = CARTESIAN_POINT ( 'NONE',  ( 2.500000000000000000, 1.768423874527822681, -1.021000000000002794 ) ) ;
#5311 = AXIS2_PLACEMENT_3D ( 'NONE', #6166, #4127, #864 ) ;
#5312 = PRODUCT_RELATED_PRODUCT_CATEGORY ( 'part', '', ( #8583 ) ) ;
#5313 = CARTESIAN_POINT ( 'NONE',  ( 181.0000000000000000, -4.999999999999998224, 145.0000000000000284 ) ) ;
#5314 = VECTOR ( 'NONE', #6428, 1000.000000000000000 ) ;
#5315 = STYLED_ITEM ( 'NONE', ( #3039 ), #6044 ) ;
#5316 = PLANE ( 'NONE',  #183 ) ;
#5317 = CARTESIAN_POINT ( 'NONE',  ( 3.999999999999999112, 1.941961291383486277, -0.3515519931180248192 ) ) ;
#5318 = VECTOR ( 'NONE', #1046, 1000.000000000000000 ) ;
#5319 = CARTESIAN_POINT ( 'NONE',  ( 0.000000000000000000, 0.000000000000000000, -5.000000000000000000 ) ) ;
#5320 = AXIS2_PLACEMENT_3D ( 'NONE', #5716, #3031, #5758 ) ;
#5321 = PLANE ( 'NONE',  #2625 ) ;
#5322 = DIRECTION ( 'NONE',  ( -1.734723475976806848E-16, 1.000000000000000000, 0.000000000000000000 ) ) ;
#5323 =( GEOMETRIC_REPRESENTATION_CONTEXT ( 3 ) GLOBAL_UNCERTAINTY_ASSIGNED_CONTEXT ( ( #5371 ) ) GLOBAL_UNIT_ASSIGNED_CONTEXT ( ( #5973, #4543, #4504 ) ) REPRESENTATION_CONTEXT ( 'NONE', 'WORKASPACE' ) );
#5324 = ORIENTED_EDGE ( 'NONE', *, *, #4261, .F. ) ;
#5325 = EDGE_LOOP ( 'NONE', ( #1347, #1453, #1960, #1887, #3603, #7087 ) ) ;
#5326 = ORIENTED_EDGE ( 'NONE', *, *, #7179, .T. ) ;
#5327 = DIRECTION ( 'NONE',  ( 0.000000000000000000, 0.000000000000000000, 1.000000000000000000 ) ) ;
#5328 = ADVANCED_FACE ( 'NONE', ( #2917 ), #8195, .T. ) ;
#5329 = DIRECTION ( 'NONE',  ( 1.000000000000000000, 0.000000000000000000, 0.000000000000000000 ) ) ;
#5330 = VECTOR ( 'NONE', #6150, 1000.000000000000000 ) ;
#5331 = EDGE_CURVE ( 'NONE', #2415, #3580, #3615, .T. ) ;
#5332 = ORIENTED_EDGE ( 'NONE', *, *, #8064, .F. ) ;
#5333 = CARTESIAN_POINT ( 'NONE',  ( -5.000000000000000000, -5.000000000000000000, 140.0000000000000000 ) ) ;
#5334 = ADVANCED_FACE ( 'NONE', ( #833 ), #6263, .T. ) ;
#5335 = VERTEX_POINT ( 'NONE', #1441 ) ;
#5336 = CARTESIAN_POINT ( 'NONE',  ( 0.000000000000000000, 0.000000000000000000, -4.694516984716113228 ) ) ;
#5337 = CARTESIAN_POINT ( 'NONE',  ( 444.9999999999999432, 5.000000000000000000, 140.0000000000000000 ) ) ;
#5338 = CARTESIAN_POINT ( 'NONE',  ( 440.0000000000000000, -29.99999999999999289, 18.96857495968451346 ) ) ;
#5339 = CARTESIAN_POINT ( 'NONE',  ( -1.144235203016679359, -3.958177651039096911, -0.09382832055446428676 ) ) ;
#5340 = ORIENTED_EDGE ( 'NONE', *, *, #2534, .T. ) ;
#5341 = VECTOR ( 'NONE', #507, 1000.000000000000000 ) ;
#5342 = EDGE_CURVE ( 'NONE', #6725, #2200, #4746, .T. ) ;
#5343 = VERTEX_POINT ( 'NONE', #6743 ) ;
#5344 = CARTESIAN_POINT ( 'NONE',  ( 0.000000000000000000, 0.000000000000000000, 27.00000000000000711 ) ) ;
#5345 = CARTESIAN_POINT ( 'NONE',  ( 53.33333333333330017, -20.00000000000000000, 162.5000000000000853 ) ) ;
#5346 = CARTESIAN_POINT ( 'NONE',  ( 4.204115023516791005, -1.660442669500199919, -3.602151381774560068 ) ) ;
#5347 = DIRECTION ( 'NONE',  ( 1.000000000000000000, 0.000000000000000000, 0.000000000000000000 ) ) ;
#5348 = EDGE_LOOP ( 'NONE', ( #7121, #3626 ) ) ;
#5349 =( LENGTH_UNIT ( ) NAMED_UNIT ( * ) SI_UNIT ( .MILLI., .METRE. ) );
#5350 = EDGE_LOOP ( 'NONE', ( #3590, #6683, #4751, #1455 ) ) ;
#5351 = DIRECTION ( 'NONE',  ( 0.000000000000000000, 1.000000000000000000, 0.000000000000000000 ) ) ;
#5352 = AXIS2_PLACEMENT_3D ( 'NONE', #4302, #912, #7480 ) ;
#5353 = PLANE ( 'NONE',  #227 ) ;
#5354 = CARTESIAN_POINT ( 'NONE',  ( -4.999999999999998224, 135.0000000000000000, 25.00000000000000000 ) ) ;
#5355 = VERTEX_POINT ( 'NONE', #5484 ) ;
#5356 = PLANE ( 'NONE',  #7922 ) ;
#5357 = FACE_OUTER_BOUND ( 'NONE', #2725, .T. ) ;
#5358 = AXIS2_PLACEMENT_3D ( 'NONE', #7910, #6023, #1419 ) ;
#5359 = EDGE_CURVE ( 'NONE', #2080, #798, #736, .T. ) ;
#5360 = CIRCLE ( 'NONE', #1619, 20.00000000000000000 ) ;
#5361 = ADVANCED_FACE ( 'NONE', ( #3446 ), #5436, .F. ) ;
#5362 = CARTESIAN_POINT ( 'NONE',  ( 176.0000000000000000, -20.00000000000000000, -83.98142504031548583 ) ) ;
#5363 = EDGE_CURVE ( 'NONE', #1280, #7885, #1443, .T. ) ;
#5364 = FACE_OUTER_BOUND ( 'NONE', #7292, .T. ) ;
#5365 = VECTOR ( 'NONE', #4239, 1000.000000000000000 ) ;
#5366 = CARTESIAN_POINT ( 'NONE',  ( 5.000000000000000000, -5.000000000000000000, 148.0000000000000284 ) ) ;
#5367 =( NAMED_UNIT ( * ) SI_UNIT ( $, .STERADIAN. ) SOLID_ANGLE_UNIT ( ) );
#5368 = VECTOR ( 'NONE', #8329, 1000.000000000000000 ) ;
#5369 = VERTEX_POINT ( 'NONE', #1571 ) ;
#5370 = ORIENTED_EDGE ( 'NONE', *, *, #2865, .T. ) ;
#5371 = UNCERTAINTY_MEASURE_WITH_UNIT (LENGTH_MEASURE( 1.000000000000000082E-05 ), #5973, 'distance_accuracy_value', 'NONE');
#5372 = VERTEX_POINT ( 'NONE', #1484 ) ;
#5373 = DIRECTION ( 'NONE',  ( -0.000000000000000000, -0.000000000000000000, 1.000000000000000000 ) ) ;
#5374 = CARTESIAN_POINT ( 'NONE',  ( 259.0000000000000000, 5.000000000000001776, 139.9990000000000236 ) ) ;
#5375 = VECTOR ( 'NONE', #2869, 1000.000000000000000 ) ;
#5376 = EDGE_CURVE ( 'NONE', #6692, #1565, #1574, .T. ) ;
#5377 = ORIENTED_EDGE ( 'NONE', *, *, #5677, .T. ) ;
#5378 = DIRECTION ( 'NONE',  ( 0.000000000000000000, 0.000000000000000000, -1.000000000000000000 ) ) ;
#5379 = ORIENTED_EDGE ( 'NONE', *, *, #5750, .T. ) ;
#5380 = DIRECTION ( 'NONE',  ( -0.000000000000000000, -0.000000000000000000, 1.000000000000000000 ) ) ;
#5381 = CARTESIAN_POINT ( 'NONE',  ( 0.2500000000000002220, 0.000000000000000000, 4.250000000000000000 ) ) ;
#5382 = APPLICATION_PROTOCOL_DEFINITION ( 'draft international standard', 'automotive_design', 1998, #472 ) ;
#5383 = CARTESIAN_POINT ( 'NONE',  ( 0.000000000000000000, 0.000000000000000000, 148.0000000000000284 ) ) ;
#5384 = VERTEX_POINT ( 'NONE', #2835 ) ;
#5385 = EDGE_LOOP ( 'NONE', ( #3614, #5761, #8201, #4336, #8455 ) ) ;
#5386 = CARTESIAN_POINT ( 'NONE',  ( -5.000000000000000000, -5.000000000000000000, 148.0000000000000284 ) ) ;
#5387 = CARTESIAN_POINT ( 'NONE',  ( 82.99999999999998579, -4.999999999999998224, 145.0000000000000284 ) ) ;
#5388 = EDGE_CURVE ( 'NONE', #5393, #590, #8152, .T. ) ;
#5389 = LINE ( 'NONE', #4739, #517 ) ;
#5390 = CARTESIAN_POINT ( 'NONE',  ( 2.807080416178989513, -3.225969019225150003, -3.502507215260505014 ) ) ;
#5391 = ORIENTED_EDGE ( 'NONE', *, *, #2769, .T. ) ;
#5392 = DIRECTION ( 'NONE',  ( -0.000000000000000000, -0.000000000000000000, -1.000000000000000000 ) ) ;
#5393 = VERTEX_POINT ( 'NONE', #6830 ) ;
#5394 = CARTESIAN_POINT ( 'NONE',  ( -4.000000000000000000, 2.309401076758498483, -5.000000000000000000 ) ) ;
#5395 = ADVANCED_FACE ( 'NONE', ( #877 ), #6177, .F. ) ;
#5396 = VECTOR ( 'NONE', #4008, 1000.000000000000000 ) ;
#5397 = EDGE_CURVE ( 'NONE', #5626, #7609, #8393, .T. ) ;
#5398 = CARTESIAN_POINT ( 'NONE',  ( 20.00000000000000000, 175.0000000000000284, 0.000000000000000000 ) ) ;
#5399 = DIRECTION ( 'NONE',  ( 1.000000000000000000, 0.000000000000000000, 0.000000000000000000 ) ) ;
#5400 = ORIENTED_EDGE ( 'NONE', *, *, #1093, .T. ) ;
#5401 = DIRECTION ( 'NONE',  ( 0.000000000000000000, 0.000000000000000000, 1.000000000000000000 ) ) ;
#5402 = CIRCLE ( 'NONE', #5686, 10.00000000000000000 ) ;
#5403 = CARTESIAN_POINT ( 'NONE',  ( -5.000000000000001776, 5.000000000000001776, 140.0000000000000000 ) ) ;
#5404 = FACE_OUTER_BOUND ( 'NONE', #159, .T. ) ;
#5405 = VECTOR ( 'NONE', #5188, 1000.000000000000000 ) ;
#5406 = CARTESIAN_POINT ( 'NONE',  ( 82.99999999999998579, -4.999999999999998224, 139.9990000000000236 ) ) ;
#5407 = DIRECTION ( 'NONE',  ( 0.000000000000000000, 0.000000000000000000, -1.000000000000000000 ) ) ;
#5408 = CARTESIAN_POINT ( 'NONE',  ( 0.000000000000000000, 0.000000000000000000, 27.00000000000001066 ) ) ;
#5409 = EDGE_CURVE ( 'NONE', #489, #6262, #2554, .T. ) ;
#5410 = ORIENTED_EDGE ( 'NONE', *, *, #235, .T. ) ;
#5411 = ORIENTED_EDGE ( 'NONE', *, *, #7205, .T. ) ;
#5412 = EDGE_LOOP ( 'NONE', ( #1698, #350, #3287, #2715 ) ) ;
#5413 = LINE ( 'NONE', #2894, #3118 ) ;
#5414 = CIRCLE ( 'NONE', #126, 10.00000000000000000 ) ;
#5415 = ADVANCED_BREP_SHAPE_REPRESENTATION ( '', ( #7589, #594 ), #8234 ) ;
#5416 = ORIENTED_EDGE ( 'NONE', *, *, #3323, .T. ) ;
#5417 = DIRECTION ( 'NONE',  ( 1.000000000000000000, -1.734723475976806848E-16, 0.000000000000000000 ) ) ;
#5418 = EDGE_LOOP ( 'NONE', ( #3684, #2804, #3217, #1946 ) ) ;
#5419 = CARTESIAN_POINT ( 'NONE',  ( 2.805705207896068476, -3.226868319750173075, -3.503898532754370354 ) ) ;
#5420 = CARTESIAN_POINT ( 'NONE',  ( 434.9999999999999432, 5.000000000000001776, 139.9990000000000236 ) ) ;
#5421 = SHAPE_DEFINITION_REPRESENTATION ( #6135, #7993 ) ;
#5422 = PRODUCT_RELATED_PRODUCT_CATEGORY ( 'part', '', ( #8104 ) ) ;
#5423 = LINE ( 'NONE', #6111, #6974 ) ;
#5424 = VERTEX_POINT ( 'NONE', #1133 ) ;
#5425 = ORIENTED_EDGE ( 'NONE', *, *, #7926, .F. ) ;
#5426 = CARTESIAN_POINT ( 'NONE',  ( -4.024497503033519941, -2.323544716729390558, -3.572167766733381544 ) ) ;
#5427 = DIRECTION ( 'NONE',  ( 0.000000000000000000, 0.000000000000000000, -1.000000000000000000 ) ) ;
#5428 = DIRECTION ( 'NONE',  ( -0.000000000000000000, 1.000000000000000000, -0.000000000000000000 ) ) ;
#5429 = CARTESIAN_POINT ( 'NONE',  ( 1.391697335622810172, 4.043246145443375461, -3.503898532754365913 ) ) ;
#5430 = ORIENTED_EDGE ( 'NONE', *, *, #7571, .F. ) ;
#5431 =( NAMED_UNIT ( * ) SI_UNIT ( $, .STERADIAN. ) SOLID_ANGLE_UNIT ( ) );
#5432 = AXIS2_PLACEMENT_3D ( 'NONE', #5692, #3697, #7791 ) ;
#5433 = DIRECTION ( 'NONE',  ( -0.000000000000000000, -0.000000000000000000, -1.000000000000000000 ) ) ;
#5434 = ORIENTED_EDGE ( 'NONE', *, *, #7407, .F. ) ;
#5435 = ORIENTED_EDGE ( 'NONE', *, *, #3282, .F. ) ;
#5436 = PLANE ( 'NONE',  #5182 ) ;
#5437 = PRODUCT_DEFINITION_FORMATION_WITH_SPECIFIED_SOURCE ( 'ANY', '', #1270, .NOT_KNOWN. ) ;
#5438 = CARTESIAN_POINT ( 'NONE',  ( 0.000000000000000000, -20.00000000000000000, -157.5000000000000284 ) ) ;
#5439 = EDGE_CURVE ( 'NONE', #7313, #2500, #1833, .T. ) ;
#5440 = CARTESIAN_POINT ( 'NONE',  ( 0.000000000000000000, 0.000000000000000000, 120.0000000000000142 ) ) ;
#5441 = VERTEX_POINT ( 'NONE', #4438 ) ;
#5442 = FACE_BOUND ( 'NONE', #7655, .T. ) ;
#5443 = EDGE_CURVE ( 'NONE', #8141, #3913, #6005, .T. ) ;
#5444 = DIRECTION ( 'NONE',  ( 0.000000000000000000, 0.000000000000000000, -1.000000000000000000 ) ) ;
#5445 = VECTOR ( 'NONE', #1811, 1000.000000000000000 ) ;
#5446 = EDGE_CURVE ( 'NONE', #4682, #4177, #430, .T. ) ;
#5447 = CARTESIAN_POINT ( 'NONE',  ( -5.384454397937118664, 6.702023979852544604E-16, -5.000000000000000000 ) ) ;
#5448 = AXIS2_PLACEMENT_3D ( 'NONE', #4976, #7635, #1015 ) ;
#5449 = DIRECTION ( 'NONE',  ( -0.000000000000000000, -0.000000000000000000, 1.000000000000000000 ) ) ;
#5450 = VECTOR ( 'NONE', #2372, 1000.000000000000000 ) ;
#5451 = CARTESIAN_POINT ( 'NONE',  ( -10.00000000000000000, 1.224646799147353256E-15, 7.000000000000006217 ) ) ;
#5452 = DIRECTION ( 'NONE',  ( 1.000000000000000000, 0.000000000000000000, 0.000000000000000000 ) ) ;
#5453 = EDGE_LOOP ( 'NONE', ( #141, #8214 ) ) ;
#5454 = ORIENTED_EDGE ( 'NONE', *, *, #189, .T. ) ;
#5455 = VERTEX_POINT ( 'NONE', #8457 ) ;
#5456 = DIRECTION ( 'NONE',  ( 0.000000000000000000, 0.000000000000000000, 1.000000000000000000 ) ) ;
#5457 = VECTOR ( 'NONE', #7919, 1000.000000000000000 ) ;
#5458 = SURFACE_STYLE_FILL_AREA ( #3465 ) ;
#5459 = EDGE_CURVE ( 'NONE', #7335, #3184, #2130, .T. ) ;
#5460 = ORIENTED_EDGE ( 'NONE', *, *, #8070, .F. ) ;
#5461 = CARTESIAN_POINT ( 'NONE',  ( -20.00000000000000000, 175.0000000000000284, 5.000000000000000000 ) ) ;
#5462 = ORIENTED_EDGE ( 'NONE', *, *, #7639, .F. ) ;
#5463 = CARTESIAN_POINT ( 'NONE',  ( 0.000000000000000000, 0.000000000000000000, 120.0000000000000142 ) ) ;
#5464 = CARTESIAN_POINT ( 'NONE',  ( 259.0000000000000000, 5.000000000000001776, 140.0000000000000000 ) ) ;
#5465 = ITEM_DEFINED_TRANSFORMATION ( 'NONE', 'NONE', #1262,  #594 ) ;
#5466 = FACE_OUTER_BOUND ( 'NONE', #7755, .T. ) ;
#5467 = ORIENTED_EDGE ( 'NONE', *, *, #235, .F. ) ;
#5468 = ORIENTED_EDGE ( 'NONE', *, *, #4313, .F. ) ;
#5469 = VECTOR ( 'NONE', #7813, 1000.000000000000000 ) ;
#5470 = CARTESIAN_POINT ( 'NONE',  ( 219.9999999999999716, -25.00000000000000000, 162.5000000000000853 ) ) ;
#5471 = DIRECTION ( 'NONE',  ( 0.000000000000000000, 0.4999999999999993339, -0.8660254037844390407 ) ) ;
#5472 = EDGE_CURVE ( 'NONE', #5002, #7290, #6959, .T. ) ;
#5473 = EDGE_CURVE ( 'NONE', #958, #5730, #7624, .T. ) ;
#5474 = EDGE_CURVE ( 'NONE', #337, #3347, #7050, .T. ) ;
#5475 = CIRCLE ( 'NONE', #46, 2.649999999999985700 ) ;
#5476 = CARTESIAN_POINT ( 'NONE',  ( 0.000000000000000000, 0.000000000000000000, -4.974599999999998801 ) ) ;
#5477 = DIRECTION ( 'NONE',  ( 0.000000000000000000, 0.000000000000000000, 1.000000000000000000 ) ) ;
#5478 = ORIENTED_EDGE ( 'NONE', *, *, #2229, .F. ) ;
#5479 = DIRECTION ( 'NONE',  ( -1.000000000000000000, -0.000000000000000000, -0.000000000000000000 ) ) ;
#5480 = SHAPE_REPRESENTATION_RELATIONSHIP ( 'NONE' , 'NONE' ,  #7686, #3979 ) ;
#5481 = DIRECTION ( 'NONE',  ( -0.000000000000000000, -0.000000000000000000, 1.000000000000000000 ) ) ;
#5482 = VERTEX_POINT ( 'NONE', #3702 ) ;
#5483 = EDGE_LOOP ( 'NONE', ( #4285, #8279, #4072, #690 ) ) ;
#5484 = CARTESIAN_POINT ( 'NONE',  ( 0.000000000000000000, 5.051668046482832750E-16, -4.000000000000000000 ) ) ;
#5485 = LINE ( 'NONE', #6661, #5194 ) ;
#5486 = DIRECTION ( 'NONE',  ( 0.000000000000000000, 0.000000000000000000, 1.000000000000000000 ) ) ;
#5487 = DIRECTION ( 'NONE',  ( -1.000000000000000000, 0.000000000000000000, 0.000000000000000000 ) ) ;
#5488 = VERTEX_POINT ( 'NONE', #3742 ) ;
#5489 = LINE ( 'NONE', #4231, #2083 ) ;
#5490 = SHAPE_REPRESENTATION_RELATIONSHIP ( 'NONE' , 'NONE' ,  #1479, #1176 ) ;
#5491 = CARTESIAN_POINT ( 'NONE',  ( 2.500000000000000000, 2.357898499370433054, -1.951563910473907981E-15 ) ) ;
#5492 = DIRECTION ( 'NONE',  ( 0.000000000000000000, 0.000000000000000000, 1.000000000000000000 ) ) ;
#5493 = AXIS2_PLACEMENT_3D ( 'NONE', #3643, #2354, #3691 ) ;
#5494 = LINE ( 'NONE', #6927, #3481 ) ;
#5495 = EDGE_CURVE ( 'NONE', #542, #1660, #6704, .T. ) ;
#5496 = CARTESIAN_POINT ( 'NONE',  ( 0.1410422978106145031, -4.700232962125109104, -3.687027686973628704 ) ) ;
#5497 = DIRECTION ( 'NONE',  ( 0.000000000000000000, -0.000000000000000000, 1.000000000000000000 ) ) ;
#5498 = ORIENTED_EDGE ( 'NONE', *, *, #4565, .F. ) ;
#5499 = AXIS2_PLACEMENT_3D ( 'NONE', #6158, #1598, #4118 ) ;
#5500 = VERTEX_POINT ( 'NONE', #481 ) ;
#5501 = EDGE_LOOP ( 'NONE', ( #4709, #7084 ) ) ;
#5502 = LINE ( 'NONE', #1413, #5330 ) ;
#5503 = CIRCLE ( 'NONE', #4263, 2.055000000000000160 ) ;
#5504 = VECTOR ( 'NONE', #905, 1000.000000000000000 ) ;
#5505 = VERTEX_POINT ( 'NONE', #2452 ) ;
#5506 = DIRECTION ( 'NONE',  ( -0.000000000000000000, 1.000000000000000000, -0.000000000000000000 ) ) ;
#5507 = ORIENTED_EDGE ( 'NONE', *, *, #2458, .T. ) ;
#5508 = DIRECTION ( 'NONE',  ( 1.000000000000000000, 0.000000000000000000, 0.000000000000000000 ) ) ;
#5509 = CARTESIAN_POINT ( 'NONE',  ( -20.00000000000000000, 135.0000000000000000, 40.00000000000000000 ) ) ;
#5510 = ITEM_DEFINED_TRANSFORMATION ( 'NONE', 'NONE', #6833,  #594 ) ;
#5511 = ORIENTED_EDGE ( 'NONE', *, *, #2023, .T. ) ;
#5512 = ORIENTED_EDGE ( 'NONE', *, *, #2747, .F. ) ;
#5513 = AXIS2_PLACEMENT_3D ( 'NONE', #5016, #8427, #2980 ) ;
#5515 = AXIS2_PLACEMENT_3D ( 'NONE', #6836, #2920, #7492 ) ;
#5514 = DIRECTION ( 'NONE',  ( 1.000000000000000000, 0.000000000000000000, 0.000000000000000000 ) ) ;
#5516 = DIRECTION ( 'NONE',  ( 1.000000000000000000, 0.000000000000000000, 0.000000000000000000 ) ) ;
#5517 = CARTESIAN_POINT ( 'NONE',  ( -6.473970235329672780E-16, -4.862606272033106691, -3.745885042887442395 ) ) ;
#5518 = DIRECTION ( 'NONE',  ( -1.734723475976806848E-16, 1.000000000000000000, 0.000000000000000000 ) ) ;
#5519 = ORIENTED_EDGE ( 'NONE', *, *, #8328, .T. ) ;
#5520 = EDGE_CURVE ( 'NONE', #2221, #1967, #6349, .T. ) ;
#5521 = DIRECTION ( 'NONE',  ( 1.000000000000000000, 0.000000000000000000, 0.000000000000000000 ) ) ;
#5522 = EDGE_CURVE ( 'NONE', #7213, #6477, #5737, .T. ) ;
#5523 = ORIENTED_EDGE ( 'NONE', *, *, #5995, .T. ) ;
#5524 = CARTESIAN_POINT ( 'NONE',  ( -2.725741868435985094, 3.045094352034055429, -3.220599429844047012 ) ) ;
#5525 = AXIS2_PLACEMENT_3D ( 'NONE', #3318, #83, #2714 ) ;
#5526 = CARTESIAN_POINT ( 'NONE',  ( -2.059999999999998721, 2.522772406243545965E-16, -0.3080913168122742518 ) ) ;
#5527 = APPLICATION_CONTEXT ( 'automotive_design' ) ;
#5528 = LINE ( 'NONE', #4880, #5793 ) ;
#5529 = FACE_OUTER_BOUND ( 'NONE', #1049, .T. ) ;
#5530 = ORIENTED_EDGE ( 'NONE', *, *, #5641, .T. ) ;
#5531 = CARTESIAN_POINT ( 'NONE',  ( -4.211140560182196957, 2.431303136016537803, -3.745885042887433514 ) ) ;
#5532 = CARTESIAN_POINT ( 'NONE',  ( 386.6666666666666288, -14.99999999999999822, 162.5000000000000853 ) ) ;
#5533 = ADVANCED_FACE ( 'NONE', ( #8414 ), #4477, .F. ) ;
#5534 = AXIS2_PLACEMENT_3D ( 'NONE', #1710, #6399, #3059 ) ;
#5535 = CARTESIAN_POINT ( 'NONE',  ( -5.000000000000000000, -5.000000000000000000, 148.0000000000000284 ) ) ;
#5536 = DIRECTION ( 'NONE',  ( -0.000000000000000000, -0.000000000000000000, 1.000000000000000000 ) ) ;
#5537 = DIRECTION ( 'NONE',  ( 0.000000000000000000, 0.000000000000000000, 1.000000000000000000 ) ) ;
#5538 = CARTESIAN_POINT ( 'NONE',  ( -6.259644161404860030E-16, -4.618802153517027165, -5.000000000000000000 ) ) ;
#5539 = VECTOR ( 'NONE', #5518, 1000.000000000000000 ) ;
#5540 = ORIENTED_EDGE ( 'NONE', *, *, #3492, .F. ) ;
#5541 = EDGE_LOOP ( 'NONE', ( #1482, #3311, #725, #4718 ) ) ;
#5542 = LINE ( 'NONE', #2431, #4813 ) ;
#5543 = CARTESIAN_POINT ( 'NONE',  ( 0.000000000000000000, 0.000000000000000000, 120.0000000000000142 ) ) ;
#5544 = VECTOR ( 'NONE', #5401, 1000.000000000000000 ) ;
#5545 = EDGE_LOOP ( 'NONE', ( #3963, #1955 ) ) ;
#5546 = CARTESIAN_POINT ( 'NONE',  ( 264.0000000000000000, -20.00000000000000000, -51.43142504031546025 ) ) ;
#5547 = EDGE_CURVE ( 'NONE', #6181, #437, #387, .T. ) ;
#5548 = VERTEX_POINT ( 'NONE', #5088 ) ;
#5549 = CARTESIAN_POINT ( 'NONE',  ( -5.000000000000000000, -5.000000000000000000, 148.0000000000000284 ) ) ;
#5550 = LINE ( 'NONE', #326, #5644 ) ;
#5551 = APPLICATION_PROTOCOL_DEFINITION ( 'draft international standard', 'automotive_design', 1998, #2585 ) ;
#5552 = CYLINDRICAL_SURFACE ( 'NONE', #301, 2.649999999999985700 ) ;
#5553 = ORIENTED_EDGE ( 'NONE', *, *, #8262, .F. ) ;
#5554 = ORIENTED_EDGE ( 'NONE', *, *, #5665, .F. ) ;
#5555 = CARTESIAN_POINT ( 'NONE',  ( -5.000000000000000000, -5.000000000000000000, 148.0000000000000284 ) ) ;
#5556 = ADVANCED_FACE ( 'NONE', ( #3179 ), #3054, .F. ) ;
#5557 = LINE ( 'NONE', #7522, #3113 ) ;
#5558 = DIRECTION ( 'NONE',  ( 0.000000000000000000, 0.000000000000000000, 1.000000000000000000 ) ) ;
#5559 = DIRECTION ( 'NONE',  ( -1.000000000000000000, -0.000000000000000000, -0.000000000000000000 ) ) ;
#5560 = ORIENTED_EDGE ( 'NONE', *, *, #3966, .T. ) ;
#5561 = DIRECTION ( 'NONE',  ( 0.000000000000000000, 0.000000000000000000, 1.000000000000000000 ) ) ;
#5562 = CARTESIAN_POINT ( 'NONE',  ( 5.000000000000000000, 5.000000000000000000, -0.9999999999999940048 ) ) ;
#5563 = EDGE_LOOP ( 'NONE', ( #2871, #4938, #41, #8264 ) ) ;
#5564 = DIRECTION ( 'NONE',  ( 0.000000000000000000, -0.000000000000000000, -1.000000000000000000 ) ) ;
#5565 = DIRECTION ( 'NONE',  ( 0.000000000000000000, -0.5000000000000011102, -0.8660254037844379305 ) ) ;
#5566 = ADVANCED_FACE ( 'NONE', ( #7089 ), #5817, .F. ) ;
#5567 = CARTESIAN_POINT ( 'NONE',  ( 5.200000000000002842, 0.000000000000000000, 2.500000000000000888 ) ) ;
#5568 = PLANE ( 'NONE',  #5534 ) ;
#5569 = ORIENTED_EDGE ( 'NONE', *, *, #508, .T. ) ;
#5570 = EDGE_CURVE ( 'NONE', #8118, #2774, #8325, .T. ) ;
#5571 = FACE_BOUND ( 'NONE', #2765, .T. ) ;
#5572 = CARTESIAN_POINT ( 'NONE',  ( 347.0000000000000000, -4.999999999999998224, 145.0000000000000284 ) ) ;
#5573 = FACE_OUTER_BOUND ( 'NONE', #696, .T. ) ;
#5574 = LINE ( 'NONE', #2336, #2802 ) ;
#5575 = PRODUCT_RELATED_PRODUCT_CATEGORY ( 'part', '', ( #6621 ) ) ;
#5576 = DIRECTION ( 'NONE',  ( 0.000000000000000000, 1.000000000000000000, 0.000000000000000000 ) ) ;
#5577 = CARTESIAN_POINT ( 'NONE',  ( 0.000000000000000000, -2.357898499370432610, 3.252606517456513302E-15 ) ) ;
#5578 = PRODUCT_DEFINITION_FORMATION_WITH_SPECIFIED_SOURCE ( 'ANY', '', #6690, .NOT_KNOWN. ) ;
#5579 = ORIENTED_EDGE ( 'NONE', *, *, #1094, .F. ) ;
#5580 = PRESENTATION_LAYER_ASSIGNMENT (  '', '', ( #7816 ) ) ;
#5581 = ORIENTED_EDGE ( 'NONE', *, *, #7913, .T. ) ;
#5582 = ORIENTED_EDGE ( 'NONE', *, *, #6651, .F. ) ;
#5583 = AXIS2_PLACEMENT_3D ( 'NONE', #7327, #500, #7195 ) ;
#5584 = CARTESIAN_POINT ( 'NONE',  ( -5.000000000000000000, -5.000000000000000000, -135.0000000000000000 ) ) ;
#5585 = DIRECTION ( 'NONE',  ( 0.000000000000000000, 1.000000000000000000, -1.471414886128461471E-15 ) ) ;
#5586 = PRODUCT_DEFINITION_SHAPE ( 'NONE', 'NONE',  #8618 ) ;
#5587 = AXIS2_PLACEMENT_3D ( 'NONE', #7145, #6491, #7765 ) ;
#5588 = ORIENTED_EDGE ( 'NONE', *, *, #4372, .T. ) ;
#5589 = PLANE ( 'NONE',  #5499 ) ;
#5590 = ORIENTED_EDGE ( 'NONE', *, *, #2587, .F. ) ;
#5591 = SHAPE_REPRESENTATION_RELATIONSHIP ( 'NONE' , 'NONE' ,  #2707, #6044 ) ;
#5592 = CARTESIAN_POINT ( 'NONE',  ( 0.000000000000000000, 0.000000000000000000, -191.5685424949238325 ) ) ;
#5593 =( NAMED_UNIT ( * ) PLANE_ANGLE_UNIT ( ) SI_UNIT ( $, .RADIAN. ) );
#5594 = VERTEX_POINT ( 'NONE', #1254 ) ;
#5595 = EDGE_CURVE ( 'NONE', #2406, #3508, #2965, .T. ) ;
#5596 = AXIS2_PLACEMENT_3D ( 'NONE', #2322, #4352, #2408 ) ;
#5597 = ORIENTED_EDGE ( 'NONE', *, *, #1244, .F. ) ;
#5598 = CARTESIAN_POINT ( 'NONE',  ( 5.000000000000000000, -5.000000000000000000, 148.0000000000000284 ) ) ;
#5599 = AXIS2_PLACEMENT_3D ( 'NONE', #3381, #1990, #5242 ) ;
#5600 = DIRECTION ( 'NONE',  ( 0.000000000000000000, 0.000000000000000000, 1.000000000000000000 ) ) ;
#5601 = EDGE_CURVE ( 'NONE', #3580, #4350, #3305, .T. ) ;
#5602 = EDGE_CURVE ( 'NONE', #1324, #5384, #7261, .T. ) ;
#5603 = LINE ( 'NONE', #6821, #6186 ) ;
#5604 = CARTESIAN_POINT ( 'NONE',  ( -20.00000000000000000, 2.449293598294706513E-15, 120.0000000000000142 ) ) ;
#5605 = ORIENTED_EDGE ( 'NONE', *, *, #1922, .T. ) ;
#5606 = EDGE_CURVE ( 'NONE', #1549, #3209, #6686, .T. ) ;
#5607 = VECTOR ( 'NONE', #4376, 1000.000000000000000 ) ;
#5608 = AXIS2_PLACEMENT_3D ( 'NONE', #5020, #1111, #4941 ) ;
#5609 = DIRECTION ( 'NONE',  ( -1.000000000000000000, 0.000000000000000000, -0.000000000000000000 ) ) ;
#5610 = ORIENTED_EDGE ( 'NONE', *, *, #781, .F. ) ;
#5611 = ORIENTED_EDGE ( 'NONE', *, *, #4391, .T. ) ;
#5612 = DIRECTION ( 'NONE',  ( 1.000000000000000000, -1.734723475976806848E-16, 0.000000000000000000 ) ) ;
#5613 = DIRECTION ( 'NONE',  ( -0.8191520442889875797, 1.003171929053519570E-16, 0.5735764363510522656 ) ) ;
#5614 = AXIS2_PLACEMENT_3D ( 'NONE', #6458, #7157, #5834 ) ;
#5615 = LINE ( 'NONE', #6312, #4824 ) ;
#5616 = DIRECTION ( 'NONE',  ( -0.000000000000000000, -0.000000000000000000, 1.000000000000000000 ) ) ;
#5617 = ORIENTED_EDGE ( 'NONE', *, *, #7749, .T. ) ;
#5618 = DIRECTION ( 'NONE',  ( 0.000000000000000000, 0.000000000000000000, -1.000000000000000000 ) ) ;
#5619 = APPLICATION_PROTOCOL_DEFINITION ( 'draft international standard', 'automotive_design', 1998, #5959 ) ;
#5620 = VECTOR ( 'NONE', #2364, 1000.000000000000000 ) ;
#5621 = CARTESIAN_POINT ( 'NONE',  ( -5.000000000000000000, -5.000000000000000000, 140.0000000000000000 ) ) ;
#5622 = FACE_OUTER_BOUND ( 'NONE', #7487, .T. ) ;
#5623 = CYLINDRICAL_SURFACE ( 'NONE', #3895, 10.00000000000000000 ) ;
#5624 = DIRECTION ( 'NONE',  ( -1.000000000000000000, 0.000000000000000000, -0.000000000000000000 ) ) ;
#5625 = LINE ( 'NONE', #4370, #6619 ) ;
#5626 = VERTEX_POINT ( 'NONE', #5987 ) ;
#5627 = ORIENTED_EDGE ( 'NONE', *, *, #4702, .T. ) ;
#5628 = ADVANCED_FACE ( 'NONE', ( #6556 ), #3394, .T. ) ;
#5629 = EDGE_CURVE ( 'NONE', #478, #8592, #3263, .T. ) ;
#5630 = ORIENTED_EDGE ( 'NONE', *, *, #2892, .F. ) ;
#5631 = LINE ( 'NONE', #5715, #4227 ) ;
#5632 = CARTESIAN_POINT ( 'NONE',  ( -5.000000000000001776, 5.000000000000001776, -105.9999999999999858 ) ) ;
#5633 = ORIENTED_EDGE ( 'NONE', *, *, #3009, .F. ) ;
#5634 = CONICAL_SURFACE ( 'NONE', #5218, 4.000000000000000000, 0.8911886515913786111 ) ;
#5635 = SURFACE_STYLE_USAGE ( .BOTH. , #1730 ) ;
#5636 = EDGE_LOOP ( 'NONE', ( #6220, #4816, #8183, #4192 ) ) ;
#5637 = CARTESIAN_POINT ( 'NONE',  ( 10.00000000000000000, 0.000000000000000000, 120.0000000000000284 ) ) ;
#5638 = ORIENTED_EDGE ( 'NONE', *, *, #7248, .F. ) ;
#5639 = VERTEX_POINT ( 'NONE', #7303 ) ;
#5640 = LINE ( 'NONE', #1739, #8400 ) ;
#5641 = EDGE_CURVE ( 'NONE', #5237, #1635, #7175, .T. ) ;
#5642 = CARTESIAN_POINT ( 'NONE',  ( 136.6666666666666288, -15.00000000000000000, 159.8500000000001080 ) ) ;
#5643 = AXIS2_PLACEMENT_3D ( 'NONE', #988, #4458, #3076 ) ;
#5644 = VECTOR ( 'NONE', #1734, 1000.000000000000000 ) ;
#5645 = CARTESIAN_POINT ( 'NONE',  ( 5.000000000000004441, 5.204748896376250699E-16, -4.250000000000000000 ) ) ;
#5646 = CARTESIAN_POINT ( 'NONE',  ( -2.000000000000002665, -3.464101615137770374, -3.142992957459237680 ) ) ;
#5647 = ORIENTED_EDGE ( 'NONE', *, *, #3203, .F. ) ;
#5648 = VECTOR ( 'NONE', #7330, 1000.000000000000000 ) ;
#5649 = AXIS2_PLACEMENT_3D ( 'NONE', #569, #7808, #7059 ) ;
#5650 = DIRECTION ( 'NONE',  ( 1.000000000000000000, 0.000000000000000000, 0.000000000000000000 ) ) ;
#5651 = CYLINDRICAL_SURFACE ( 'NONE', #6663, 2.649999999999993694 ) ;
#5652 = EDGE_LOOP ( 'NONE', ( #8151, #1927, #2309, #3261 ) ) ;
#5653 = ORIENTED_EDGE ( 'NONE', *, *, #7670, .F. ) ;
#5654 = DIRECTION ( 'NONE',  ( 1.000000000000000000, 0.000000000000000000, 0.000000000000000000 ) ) ;
#5655 = B_SPLINE_CURVE_WITH_KNOTS ( 'NONE', 3,
 ( #4559, #2615, #1434, #652, #110, #7217 ),
 .UNSPECIFIED., .F., .F.,
 ( 4, 2, 4 ),
 ( 0.002365888236227967761, 0.003551327329835077609, 0.004736766423442186590 ),
 .UNSPECIFIED. ) ;
#5656 = LINE ( 'NONE', #8458, #5620 ) ;
#5657 = DIRECTION ( 'NONE',  ( 0.000000000000000000, -0.5000000000000011102, -0.8660254037844379305 ) ) ;
#5658 = CARTESIAN_POINT ( 'NONE',  ( 0.000000000000000000, 0.000000000000000000, 120.0000000000000284 ) ) ;
#5659 = ORIENTED_EDGE ( 'NONE', *, *, #5178, .F. ) ;
#5660 = CARTESIAN_POINT ( 'NONE',  ( 10.00000000000000000, 0.000000000000000000, -63.99999999999997158 ) ) ;
#5661 =( NAMED_UNIT ( * ) SI_UNIT ( $, .STERADIAN. ) SOLID_ANGLE_UNIT ( ) );
#5662 = ORIENTED_EDGE ( 'NONE', *, *, #7637, .T. ) ;
#5663 = PRODUCT_DEFINITION_SHAPE ( 'NONE', 'NONE',  #8635 ) ;
#5664 = CARTESIAN_POINT ( 'NONE',  ( -0.1410422978106123659, 4.700232962125094893, -3.687027686973624707 ) ) ;
#5665 = EDGE_CURVE ( 'NONE', #7983, #7651, #5294, .T. ) ;
#5666 = EDGE_CURVE ( 'NONE', #8541, #8169, #2425, .T. ) ;
#5667 = DIRECTION ( 'NONE',  ( -1.000000000000000000, 1.734723475976806848E-16, -0.000000000000000000 ) ) ;
#5668 = VECTOR ( 'NONE', #570, 1000.000000000000000 ) ;
#5669 = CARTESIAN_POINT ( 'NONE',  ( 170.9999999999999716, -4.999999999999998224, 140.0000000000000000 ) ) ;
#5670 = CARTESIAN_POINT ( 'NONE',  ( 2.000000000000008882, 3.464101615137749945, 0.000000000000000000 ) ) ;
#5671 = CARTESIAN_POINT ( 'NONE',  ( -4.203934362469166963, -1.640673743454851286, -3.598432614606932756 ) ) ;
#5672 = EDGE_LOOP ( 'NONE', ( #4117, #1259 ) ) ;
#5673 = EDGE_LOOP ( 'NONE', ( #2821, #1661, #4958, #663 ) ) ;
#5674 = VERTEX_POINT ( 'NONE', #605 ) ;
#5675 = DIRECTION ( 'NONE',  ( 0.000000000000000000, 1.000000000000000000, 0.000000000000000000 ) ) ;
#5676 = DIRECTION ( 'NONE',  ( 0.000000000000000000, 0.000000000000000000, -1.000000000000000000 ) ) ;
#5677 = EDGE_CURVE ( 'NONE', #2732, #4765, #6520, .T. ) ;
#5678 = VERTEX_POINT ( 'NONE', #1961 ) ;
#5679 = DIRECTION ( 'NONE',  ( 0.000000000000000000, 0.000000000000000000, 1.000000000000000000 ) ) ;
#5680 = ORIENTED_EDGE ( 'NONE', *, *, #2892, .T. ) ;
#5681 = CARTESIAN_POINT ( 'NONE',  ( -5.000000000000001776, 5.000000000000001776, -36.00000000000000000 ) ) ;
#5682 = ITEM_DEFINED_TRANSFORMATION ( 'NONE', 'NONE', #5298,  #594 ) ;
#5683 = ORIENTED_EDGE ( 'NONE', *, *, #7899, .T. ) ;
#5684 = EDGE_LOOP ( 'NONE', ( #7918, #4597, #1023, #6893 ) ) ;
#5685 = DIRECTION ( 'NONE',  ( 0.000000000000000000, 0.000000000000000000, 1.000000000000000000 ) ) ;
#5686 = AXIS2_PLACEMENT_3D ( 'NONE', #2954, #8278, #6952 ) ;
#5687 = LINE ( 'NONE', #1693, #3383 ) ;
#5688 =( REPRESENTATION_RELATIONSHIP ('NONE','NONE', #3312, #872 ) REPRESENTATION_RELATIONSHIP_WITH_TRANSFORMATION ( #3772 )SHAPE_REPRESENTATION_RELATIONSHIP( ) );
#5689 = CARTESIAN_POINT ( 'NONE',  ( 4.000000000000000000, -2.309401076758514915, -3.433295621305383349 ) ) ;
#5690 = CARTESIAN_POINT ( 'NONE',  ( 303.3333333333333144, -15.00000000000000000, 162.5000000000000853 ) ) ;
#5691 = ORIENTED_EDGE ( 'NONE', *, *, #3454, .F. ) ;
#5692 = CARTESIAN_POINT ( 'NONE',  ( 219.9999999999999716, -10.00000000000000000, 162.5000000000000853 ) ) ;
#5693 = CARTESIAN_POINT ( 'NONE',  ( 2.500000000000000000, 1.178949249685213863, -2.042000000000001148 ) ) ;
#5694 = VERTEX_POINT ( 'NONE', #2006 ) ;
#5695 = EDGE_LOOP ( 'NONE', ( #6731, #2749, #4043, #7386 ) ) ;
#5696 = CARTESIAN_POINT ( 'NONE',  ( 0.000000000000000000, 0.000000000000000000, -63.99999999999997158 ) ) ;
#5697 = DIRECTION ( 'NONE',  ( -0.000000000000000000, 1.000000000000000000, -0.000000000000000000 ) ) ;
#5698 = VECTOR ( 'NONE', #8425, 1000.000000000000000 ) ;
#5699 = PLANE ( 'NONE',  #1323 ) ;
#5700 = DIRECTION ( 'NONE',  ( 1.000000000000000000, 0.000000000000000000, 0.000000000000000000 ) ) ;
#5701 = ADVANCED_FACE ( 'NONE', ( #1338 ), #6601, .F. ) ;
#5702 = ORIENTED_EDGE ( 'NONE', *, *, #299, .T. ) ;
#5703 = ORIENTED_EDGE ( 'NONE', *, *, #1094, .T. ) ;
#5704 = FACE_BOUND ( 'NONE', #7185, .T. ) ;
#5705 = DIRECTION ( 'NONE',  ( -1.000000000000000000, 0.000000000000000000, 0.000000000000000000 ) ) ;
#5706 = EDGE_CURVE ( 'NONE', #3371, #7420, #7256, .T. ) ;
#5707 = FACE_BOUND ( 'NONE', #5085, .T. ) ;
#5708 = DIRECTION ( 'NONE',  ( 1.000000000000000000, 0.000000000000000000, 0.000000000000000000 ) ) ;
#5709 = ADVANCED_FACE ( 'NONE', ( #2699, #5859 ), #8535, .F. ) ;
#5710 = CYLINDRICAL_SURFACE ( 'NONE', #6522, 2.649999999999985700 ) ;
#5711 = ORIENTED_EDGE ( 'NONE', *, *, #5279, .F. ) ;
#5712 = ADVANCED_FACE ( 'NONE', ( #5943 ), #3642, .T. ) ;
#5713 =( GEOMETRIC_REPRESENTATION_CONTEXT ( 3 ) GLOBAL_UNCERTAINTY_ASSIGNED_CONTEXT ( ( #8390 ) ) GLOBAL_UNIT_ASSIGNED_CONTEXT ( ( #2957, #6825, #3570 ) ) REPRESENTATION_CONTEXT ( 'NONE', 'WORKASPACE' ) );
#5714 = CARTESIAN_POINT ( 'NONE',  ( 386.6666666666666288, -20.00000000000000000, 162.5000000000000853 ) ) ;
#5715 = CARTESIAN_POINT ( 'NONE',  ( -5.000000000000001776, 5.000000000000001776, -71.99999999999998579 ) ) ;
#5716 = CARTESIAN_POINT ( 'NONE',  ( 176.0000000000000000, -20.00000000000000000, -86.63142504031547730 ) ) ;
#5717 = AXIS2_PLACEMENT_3D ( 'NONE', #5128, #3783, #1086 ) ;
#5718 = ORIENTED_EDGE ( 'NONE', *, *, #1233, .F. ) ;
#5719 = DIRECTION ( 'NONE',  ( -0.000000000000000000, -0.000000000000000000, 1.000000000000000000 ) ) ;
#5720 = ORIENTED_EDGE ( 'NONE', *, *, #4842, .T. ) ;
#5721 = CARTESIAN_POINT ( 'NONE',  ( -4.000000000000000000, 1.941961291383472732, -0.3515519931180205448 ) ) ;
#5722 = EDGE_LOOP ( 'NONE', ( #5957, #5086, #2093, #8226 ) ) ;
#5723 = ORIENTED_EDGE ( 'NONE', *, *, #2458, .F. ) ;
#5724 = EDGE_CURVE ( 'NONE', #3602, #4249, #6645, .T. ) ;
#5725 = CARTESIAN_POINT ( 'NONE',  ( 0.000000000000000000, 0.000000000000000000, 140.0000000000000000 ) ) ;
#5726 = DIRECTION ( 'NONE',  ( 1.000000000000000000, 0.000000000000000000, 0.000000000000000000 ) ) ;
#5727 = AXIS2_PLACEMENT_3D ( 'NONE', #158, #1524, #2748 ) ;
#5728 = CARTESIAN_POINT ( 'NONE',  ( -5.000000000000000000, -5.000000000000000000, -135.0000000000000000 ) ) ;
#5729 = PRODUCT_DEFINITION_SHAPE ( 'NONE', 'NONE',  #8628 ) ;
#5730 = VERTEX_POINT ( 'NONE', #7350 ) ;
#5731 = DIRECTION ( 'NONE',  ( 1.000000000000000000, 0.000000000000000000, 0.000000000000000000 ) ) ;
#5732 = CARTESIAN_POINT ( 'NONE',  ( 20.00000000000000000, 0.000000000000000000, -43.99999999999997158 ) ) ;
#5733 = EDGE_LOOP ( 'NONE', ( #6701, #2750, #1680, #8428 ) ) ;
#5734 = VERTEX_POINT ( 'NONE', #4908 ) ;
#5735 = AXIS2_PLACEMENT_3D ( 'NONE', #8005, #5852, #4513 ) ;
#5736 = EDGE_CURVE ( 'NONE', #1468, #7420, #302, .T. ) ;
#5737 = LINE ( 'NONE', #3788, #3105 ) ;
#5738 = EDGE_CURVE ( 'NONE', #8215, #133, #2977, .T. ) ;
#5739 = CARTESIAN_POINT ( 'NONE',  ( 0.6666666666666658525, -4.233901974057276085, -3.300726591567086476 ) ) ;
#5740 = VECTOR ( 'NONE', #5167, 1000.000000000000000 ) ;
#5741 = EDGE_CURVE ( 'NONE', #6638, #5343, #2008, .T. ) ;
#5742 = VECTOR ( 'NONE', #7038, 1000.000000000000000 ) ;
#5743 = DIRECTION ( 'NONE',  ( 0.000000000000000000, -1.000000000000000000, 1.287488025362403787E-15 ) ) ;
#5744 = DIRECTION ( 'NONE',  ( 0.000000000000000000, 1.000000000000000000, 0.000000000000000000 ) ) ;
#5745 = VERTEX_POINT ( 'NONE', #780 ) ;
#5746 =( NAMED_UNIT ( * ) SI_UNIT ( $, .STERADIAN. ) SOLID_ANGLE_UNIT ( ) );
#5747 = VERTEX_POINT ( 'NONE', #5555 ) ;
#5748 = CARTESIAN_POINT ( 'NONE',  ( -10.00000000000000000, 1.224646799147353256E-15, -135.0000000000000000 ) ) ;
#5749 = CIRCLE ( 'NONE', #6712, 2.649999999999985700 ) ;
#5750 = EDGE_CURVE ( 'NONE', #2805, #5053, #4090, .T. ) ;
#5751 = FACE_BOUND ( 'NONE', #6342, .T. ) ;
#5752 = LINE ( 'NONE', #6363, #5698 ) ;
#5753 = FACE_OUTER_BOUND ( 'NONE', #8333, .T. ) ;
#5754 = VECTOR ( 'NONE', #4130, 1000.000000000000000 ) ;
#5755 = VERTEX_POINT ( 'NONE', #2259 ) ;
#5756 = DIRECTION ( 'NONE',  ( 0.000000000000000000, 0.000000000000000000, 1.000000000000000000 ) ) ;
#5757 = DIRECTION ( 'NONE',  ( 0.000000000000000000, -1.000000000000000000, 0.000000000000000000 ) ) ;
#5758 = DIRECTION ( 'NONE',  ( 0.000000000000000000, 0.000000000000000000, 1.000000000000000000 ) ) ;
#5759 = UNCERTAINTY_MEASURE_WITH_UNIT (LENGTH_MEASURE( 1.000000000000000082E-05 ), #349, 'distance_accuracy_value', 'NONE');
#5760 = ADVANCED_FACE ( 'NONE', ( #6733 ), #3932, .T. ) ;
#5761 = ORIENTED_EDGE ( 'NONE', *, *, #6610, .F. ) ;
#5762 = CARTESIAN_POINT ( 'NONE',  ( 352.0000000000000000, -20.00000000000000000, -16.23142504031546807 ) ) ;
#5763 = EDGE_LOOP ( 'NONE', ( #938, #155, #1703, #6048 ) ) ;
#5764 = DIRECTION ( 'NONE',  ( 1.000000000000000000, 0.000000000000000000, 0.000000000000000000 ) ) ;
#5765 = FACE_OUTER_BOUND ( 'NONE', #5673, .T. ) ;
#5766 = VERTEX_POINT ( 'NONE', #198 ) ;
#5767 = ORIENTED_EDGE ( 'NONE', *, *, #2587, .T. ) ;
#5768 = DIRECTION ( 'NONE',  ( 1.000000000000000000, 0.000000000000000000, 0.000000000000000000 ) ) ;
#5769 = EDGE_CURVE ( 'NONE', #5259, #6891, #4205, .T. ) ;
#5770 = DIRECTION ( 'NONE',  ( 0.000000000000000000, 1.000000000000000000, 0.000000000000000000 ) ) ;
#5771 = EDGE_CURVE ( 'NONE', #7903, #2181, #2086, .T. ) ;
#5772 = VECTOR ( 'NONE', #3131, 1000.000000000000000 ) ;
#5773 = DIRECTION ( 'NONE',  ( -1.734723475976806848E-16, 1.000000000000000000, 0.000000000000000000 ) ) ;
#5774 = VERTEX_POINT ( 'NONE', #3559 ) ;
#5775 = DIRECTION ( 'NONE',  ( 1.000000000000000000, 8.995820158514010070E-17, 0.000000000000000000 ) ) ;
#5776 = CARTESIAN_POINT ( 'NONE',  ( -30.00000000000002842, -25.00000000000000000, 200.0000000000000000 ) ) ;
#5777 = EDGE_LOOP ( 'NONE', ( #6553, #347, #4787, #4381 ) ) ;
#5778 = ORIENTED_EDGE ( 'NONE', *, *, #7415, .T. ) ;
#5779 = VECTOR ( 'NONE', #1377, 1000.000000000000000 ) ;
#5781 = AXIS2_PLACEMENT_3D ( 'NONE', #2691, #1465, #6679 ) ;
#5780 = DIRECTION ( 'NONE',  ( 0.000000000000000000, 0.000000000000000000, -1.000000000000000000 ) ) ;
#5782 = LINE ( 'NONE', #5004, #8134 ) ;
#5783 = CIRCLE ( 'NONE', #367, 20.00000000000000000 ) ;
#5784 = CARTESIAN_POINT ( 'NONE',  ( -4.211140560182196957, 2.431303136016537803, -3.745885042887433514 ) ) ;
#5785 = EDGE_CURVE ( 'NONE', #6409, #2056, #4255, .T. ) ;
#5786 = VECTOR ( 'NONE', #7767, 1000.000000000000000 ) ;
#5787 = CARTESIAN_POINT ( 'NONE',  ( 136.6666666666666288, -20.00000000000000000, 162.5000000000000853 ) ) ;
#5788 = VERTEX_POINT ( 'NONE', #2906 ) ;
#5789 = EDGE_CURVE ( 'NONE', #6181, #6418, #2825, .T. ) ;
#5790 = VERTEX_POINT ( 'NONE', #7434 ) ;
#5791 = PLANE ( 'NONE',  #2675 ) ;
#5792 = AXIS2_PLACEMENT_3D ( 'NONE', #6407, #1807, #1147 ) ;
#5793 = VECTOR ( 'NONE', #4228, 1000.000000000000114 ) ;
#5794 = FACE_BOUND ( 'NONE', #5545, .T. ) ;
#5795 = DIRECTION ( 'NONE',  ( 0.000000000000000000, 1.000000000000000000, 0.000000000000000000 ) ) ;
#5796 = CARTESIAN_POINT ( 'NONE',  ( -30.00000000000002842, -20.00000000000000000, 140.0000000000000000 ) ) ;
#5797 = DIRECTION ( 'NONE',  ( -1.000000000000000000, 0.000000000000000000, -0.000000000000000000 ) ) ;
#5798 = EDGE_CURVE ( 'NONE', #7972, #7459, #1469, .T. ) ;
#5799 = SURFACE_SIDE_STYLE ('',( #6497 ) ) ;
#5800 = DIRECTION ( 'NONE',  ( 0.000000000000000000, 0.000000000000000000, -1.000000000000000000 ) ) ;
#5801 = CARTESIAN_POINT ( 'NONE',  ( -20.00000000000000000, 175.0000000000000284, 0.000000000000000000 ) ) ;
#5802 = ORIENTED_EDGE ( 'NONE', *, *, #5789, .T. ) ;
#5803 = CARTESIAN_POINT ( 'NONE',  ( 53.33333333333330017, -15.00000000000000000, 165.1500000000000625 ) ) ;
#5804 = VERTEX_POINT ( 'NONE', #1559 ) ;
#5805 = PLANE ( 'NONE',  #6318 ) ;
#5806 = CARTESIAN_POINT ( 'NONE',  ( -5.000000000000000000, -5.000000000000000000, 140.0000000000000000 ) ) ;
#5807 = EDGE_CURVE ( 'NONE', #1324, #8215, #6905, .T. ) ;
#5808 = DIRECTION ( 'NONE',  ( -0.000000000000000000, 1.000000000000000000, -0.000000000000000000 ) ) ;
#5809 = EDGE_CURVE ( 'NONE', #3508, #2406, #4767, .T. ) ;
#5810 = ORIENTED_EDGE ( 'NONE', *, *, #5886, .F. ) ;
#5811 = CARTESIAN_POINT ( 'NONE',  ( 0.000000000000000000, 0.000000000000000000, 0.000000000000000000 ) ) ;
#5812 = DIRECTION ( 'NONE',  ( 1.000000000000000000, -3.191891195797327272E-17, 0.000000000000000000 ) ) ;
#5813 = DIRECTION ( 'NONE',  ( -1.734723475976807587E-16, 1.000000000000000000, 0.000000000000000000 ) ) ;
#5814 = ORIENTED_EDGE ( 'NONE', *, *, #4096, .T. ) ;
#5815 = EDGE_CURVE ( 'NONE', #5747, #6448, #6777, .T. ) ;
#5816 = VERTEX_POINT ( 'NONE', #7389 ) ;
#5817 = CYLINDRICAL_SURFACE ( 'NONE', #6434, 2.649999999999993694 ) ;
#5818 = LINE ( 'NONE', #8494, #1738 ) ;
#5819 = CIRCLE ( 'NONE', #7497, 4.000000000000000000 ) ;
#5820 = DIRECTION ( 'NONE',  ( -0.000000000000000000, 1.000000000000000000, -0.000000000000000000 ) ) ;
#5821 = CARTESIAN_POINT ( 'NONE',  ( 0.000000000000000000, 0.000000000000000000, -84.56854249492380404 ) ) ;
#5822 = ORIENTED_EDGE ( 'NONE', *, *, #4313, .T. ) ;
#5823 = EDGE_LOOP ( 'NONE', ( #8412, #4651 ) ) ;
#5824 = ORIENTED_EDGE ( 'NONE', *, *, #6459, .T. ) ;
#5825 = VECTOR ( 'NONE', #1979, 1000.000000000000000 ) ;
#5826 = LINE ( 'NONE', #7015, #7254 ) ;
#5827 = EDGE_CURVE ( 'NONE', #489, #8541, #954, .T. ) ;
#5828 = EDGE_CURVE ( 'NONE', #2056, #7704, #3479, .T. ) ;
#5829 = LINE ( 'NONE', #7887, #5786 ) ;
#5830 = CARTESIAN_POINT ( 'NONE',  ( 5.000000000000000000, -5.000000000000000000, -105.9999999999999858 ) ) ;
#5831 = CARTESIAN_POINT ( 'NONE',  ( 470.0000000000000000, -20.00000000000000000, 200.0000000000000000 ) ) ;
#5832 = CARTESIAN_POINT ( 'NONE',  ( 5.000000000000000000, 5.000000000000000000, 148.0000000000000284 ) ) ;
#5833 = PLANE ( 'NONE',  #7245 ) ;
#5834 = DIRECTION ( 'NONE',  ( 0.000000000000000000, 0.000000000000000000, 1.000000000000000000 ) ) ;
#5835 = DIRECTION ( 'NONE',  ( -1.000000000000000000, -0.000000000000000000, -0.000000000000000000 ) ) ;
#5836 = EDGE_CURVE ( 'NONE', #2255, #6933, #69, .T. ) ;
#5837 = CARTESIAN_POINT ( 'NONE',  ( 4.000000000000000000, 2.309401076758497151, -3.433295621305379353 ) ) ;
#5838 = DIRECTION ( 'NONE',  ( -0.000000000000000000, 1.000000000000000000, -0.000000000000000000 ) ) ;
#5839 = PRESENTATION_LAYER_ASSIGNMENT (  '', '', ( #5986 ) ) ;
#5840 = ORIENTED_EDGE ( 'NONE', *, *, #4465, .F. ) ;
#5841 = SURFACE_STYLE_USAGE ( .BOTH. , #1863 ) ;
#5842 = LINE ( 'NONE', #7822, #3576 ) ;
#5843 = ORIENTED_EDGE ( 'NONE', *, *, #1654, .T. ) ;
#5844 = APPLICATION_CONTEXT ( 'automotive_design' ) ;
#5845 = FACE_OUTER_BOUND ( 'NONE', #2779, .T. ) ;
#5846 = PLANE ( 'NONE',  #5599 ) ;
#5847 = AXIS2_PLACEMENT_3D ( 'NONE', #6259, #7485, #8110 ) ;
#5848 = PRODUCT_DEFINITION_SHAPE ( 'NONE', 'NONE',  #8617 ) ;
#5849 = LINE ( 'NONE', #2731, #5779 ) ;
#5850 = VERTEX_POINT ( 'NONE', #6211 ) ;
#5851 = ADVANCED_FACE ( 'NONE', ( #244 ), #287, .T. ) ;
#5852 = DIRECTION ( 'NONE',  ( 0.000000000000000000, 1.000000000000000000, 0.000000000000000000 ) ) ;
#5853 = AXIS2_PLACEMENT_3D ( 'NONE', #6304, #518, #5650 ) ;
#5854 = APPLICATION_PROTOCOL_DEFINITION ( 'draft international standard', 'automotive_design', 1998, #1081 ) ;
#5855 = PLANE ( 'NONE',  #1846 ) ;
#5856 = ORIENTED_EDGE ( 'NONE', *, *, #7823, .F. ) ;
#5857 = AXIS2_PLACEMENT_3D ( 'NONE', #3240, #4415, #2254 ) ;
#5858 = VERTEX_POINT ( 'NONE', #4467 ) ;
#5859 = FACE_OUTER_BOUND ( 'NONE', #5325, .T. ) ;
#5860 = CARTESIAN_POINT ( 'NONE',  ( -20.00000000000000000, 2.449293598294706513E-15, -115.0000000000000000 ) ) ;
#5861 = VECTOR ( 'NONE', #1232, 1000.000000000000000 ) ;
#5862 = EDGE_CURVE ( 'NONE', #6418, #8491, #7079, .T. ) ;
#5863 = CARTESIAN_POINT ( 'NONE',  ( 170.9999999999999716, 5.000000000000001776, 139.9990000000000236 ) ) ;
#5864 = CIRCLE ( 'NONE', #4346, 2.649999999999985700 ) ;
#5865 = ADVANCED_FACE ( 'NONE', ( #2444 ), #7705, .F. ) ;
#5866 = DIRECTION ( 'NONE',  ( 0.000000000000000000, 0.000000000000000000, -1.000000000000000000 ) ) ;
#5867 = LINE ( 'NONE', #8540, #8057 ) ;
#5868 = ORIENTED_EDGE ( 'NONE', *, *, #249, .F. ) ;
#5869 = CIRCLE ( 'NONE', #8522, 10.00000000000000000 ) ;
#5870 = FILL_AREA_STYLE ('',( #6358 ) ) ;
#5871 = ORIENTED_EDGE ( 'NONE', *, *, #2149, .T. ) ;
#5872 = LINE ( 'NONE', #8069, #5999 ) ;
#5873 = AXIS2_PLACEMENT_3D ( 'NONE', #5047, #7796, #1050 ) ;
#5874 = VECTOR ( 'NONE', #3824, 1000.000000000000000 ) ;
#5875 = FACE_OUTER_BOUND ( 'NONE', #205, .T. ) ;
#5876 = CARTESIAN_POINT ( 'NONE',  ( 10.00000000000000000, 0.000000000000000000, 27.00000000000000711 ) ) ;
#5877 = LINE ( 'NONE', #3237, #3744 ) ;
#5878 =( NAMED_UNIT ( * ) PLANE_ANGLE_UNIT ( ) SI_UNIT ( $, .RADIAN. ) );
#5879 = VECTOR ( 'NONE', #4895, 1000.000000000000000 ) ;
#5880 = DIRECTION ( 'NONE',  ( -0.000000000000000000, 1.000000000000000000, -0.000000000000000000 ) ) ;
#5881 = CARTESIAN_POINT ( 'NONE',  ( 357.0000000000000000, 5.000000000000000000, 139.9990000000000236 ) ) ;
#5882 = CARTESIAN_POINT ( 'NONE',  ( 386.6666666666666288, -25.00000000000000000, 162.5000000000000853 ) ) ;
#5883 = VECTOR ( 'NONE', #1663, 1000.000000000000000 ) ;
#5884 = CARTESIAN_POINT ( 'NONE',  ( 4.000000000000000000, -2.309401076758514915, -5.000000000000000000 ) ) ;
#5885 = CARTESIAN_POINT ( 'NONE',  ( 88.00000000000000000, -20.00000000000000000, -121.8314250403154659 ) ) ;
#5886 = EDGE_CURVE ( 'NONE', #730, #3075, #5640, .T. ) ;
#5887 = ORIENTED_EDGE ( 'NONE', *, *, #6089, .F. ) ;
#5888 = EDGE_CURVE ( 'NONE', #6119, #8049, #7784, .T. ) ;
#5889 = APPLICATION_PROTOCOL_DEFINITION ( 'draft international standard', 'automotive_design', 1998, #5527 ) ;
#5890 = CARTESIAN_POINT ( 'NONE',  ( -1.317756351988340180, 3.857995168970202116, -0.04852650426601388955 ) ) ;
#5891 = CONTEXT_DEPENDENT_SHAPE_REPRESENTATION ( #6127, #5663 ) ;
#5892 = ORIENTED_EDGE ( 'NONE', *, *, #8445, .F. ) ;
#5893 = CARTESIAN_POINT ( 'NONE',  ( 303.3333333333333144, -20.00000000000000000, 165.1500000000000625 ) ) ;
#5894 = AXIS2_PLACEMENT_3D ( 'NONE', #7659, #377, #5685 ) ;
#5895 = CARTESIAN_POINT ( 'NONE',  ( 0.3198814748697593746, 4.434118497892183264, -0.3507732604232499107 ) ) ;
#5896 = DIRECTION ( 'NONE',  ( -1.000000000000000000, 0.000000000000000000, 0.000000000000000000 ) ) ;
#5897 = EDGE_LOOP ( 'NONE', ( #7029, #3070, #2636, #6898 ) ) ;
#5898 = CARTESIAN_POINT ( 'NONE',  ( 82.99999999999998579, 5.000000000000001776, 145.0000000000000284 ) ) ;
#5899 = ADVANCED_FACE ( 'NONE', ( #8405, #332 ), #4386, .F. ) ;
#5900 = DIRECTION ( 'NONE',  ( -1.734723475976806848E-16, 1.000000000000000000, 0.000000000000000000 ) ) ;
#5901 = ORIENTED_EDGE ( 'NONE', *, *, #3426, .F. ) ;
#5902 = ORIENTED_EDGE ( 'NONE', *, *, #3010, .T. ) ;
#5903 = CARTESIAN_POINT ( 'NONE',  ( -3.999999999999999112, 1.539600717838996324, -3.300726591567078039 ) ) ;
#5904 = DIRECTION ( 'NONE',  ( 0.000000000000000000, 0.000000000000000000, 1.000000000000000000 ) ) ;
#5905 = DIRECTION ( 'NONE',  ( -0.000000000000000000, 1.000000000000000000, -0.000000000000000000 ) ) ;
#5906 = DIRECTION ( 'NONE',  ( -0.000000000000000000, 1.000000000000000000, -0.000000000000000000 ) ) ;
#5907 = ORIENTED_EDGE ( 'NONE', *, *, #7554, .F. ) ;
#5908 = VECTOR ( 'NONE', #5743, 1000.000000000000000 ) ;
#5909 = ORIENTED_EDGE ( 'NONE', *, *, #2435, .T. ) ;
#5910 = CARTESIAN_POINT ( 'NONE',  ( 5.000000000000000000, 5.000000000000000000, 148.0000000000000284 ) ) ;
#5911 = VECTOR ( 'NONE', #237, 1000.000000000000114 ) ;
#5912 = DIRECTION ( 'NONE',  ( -0.000000000000000000, 1.000000000000000000, -0.000000000000000000 ) ) ;
#5913 = EDGE_CURVE ( 'NONE', #6448, #4522, #1692, .T. ) ;
#5914 = CARTESIAN_POINT ( 'NONE',  ( -20.00000000000000000, 175.0000000000000284, 5.000000000000000000 ) ) ;
#5915 = ORIENTED_EDGE ( 'NONE', *, *, #8595, .F. ) ;
#5916 = CARTESIAN_POINT ( 'NONE',  ( 53.33333333333330017, -25.00000000000000000, 159.8500000000001080 ) ) ;
#5917 = ADVANCED_FACE ( 'NONE', ( #7122 ), #6297, .T. ) ;
#5918 = UNCERTAINTY_MEASURE_WITH_UNIT (LENGTH_MEASURE( 1.000000000000000082E-05 ), #665, 'distance_accuracy_value', 'NONE');
#5919 = VECTOR ( 'NONE', #3717, 1000.000000000000000 ) ;
#5920 = CIRCLE ( 'NONE', #5098, 2.649999999999987477 ) ;
#5921 = ADVANCED_FACE ( 'NONE', ( #4952 ), #6426, .F. ) ;
#5922 = DIRECTION ( 'NONE',  ( -1.000000000000000000, 0.000000000000000000, 0.000000000000000000 ) ) ;
#5923 = CYLINDRICAL_SURFACE ( 'NONE', #5583, 20.00000000000000000 ) ;
#5924 = B_SPLINE_CURVE_WITH_KNOTS ( 'NONE', 3,
 ( #8145, #4215, #2261, #6907, #2867 ),
 .UNSPECIFIED., .F., .F.,
 ( 4, 1, 4 ),
 ( 0.000000000000000000, 0.002309401076758506657, 0.004618802153517013315 ),
 .UNSPECIFIED. ) ;
#5925 = FACE_OUTER_BOUND ( 'NONE', #614, .T. ) ;
#5926 = DIRECTION ( 'NONE',  ( -0.000000000000000000, 1.000000000000000000, -0.000000000000000000 ) ) ;
#5927 = LINE ( 'NONE', #7287, #5648 ) ;
#5928 = VERTEX_POINT ( 'NONE', #3044 ) ;
#5929 = ORIENTED_EDGE ( 'NONE', *, *, #1090, .F. ) ;
#5930 =( GEOMETRIC_REPRESENTATION_CONTEXT ( 3 ) GLOBAL_UNCERTAINTY_ASSIGNED_CONTEXT ( ( #7938 ) ) GLOBAL_UNIT_ASSIGNED_CONTEXT ( ( #3931, #5878, #7937 ) ) REPRESENTATION_CONTEXT ( 'NONE', 'WORKASPACE' ) );
#5931 = ORIENTED_EDGE ( 'NONE', *, *, #2210, .T. ) ;
#5932 = DIRECTION ( 'NONE',  ( -0.9284766908852593037, 0.000000000000000000, -0.3713906763541036660 ) ) ;
#5933 = CARTESIAN_POINT ( 'NONE',  ( 10.00000000000000000, 0.000000000000000000, 120.0000000000000000 ) ) ;
#5934 = EDGE_CURVE ( 'NONE', #6692, #7063, #8444, .T. ) ;
#5935 = PRODUCT_DEFINITION_CONTEXT ( 'detailed design', #5959, 'design' ) ;
#5936 = CARTESIAN_POINT ( 'NONE',  ( 0.000000000000000000, 0.000000000000000000, 120.0000000000000142 ) ) ;
#5937 = ORIENTED_EDGE ( 'NONE', *, *, #1964, .F. ) ;
#5938 = DIRECTION ( 'NONE',  ( 1.000000000000000000, 0.000000000000000000, 0.000000000000000000 ) ) ;
#5939 = DIRECTION ( 'NONE',  ( -2.081668171172168513E-17, -1.000000000000000000, 1.110223024625156540E-16 ) ) ;
#5940 = LINE ( 'NONE', #5247, #6281 ) ;
#5941 = EDGE_LOOP ( 'NONE', ( #2646, #2225 ) ) ;
#5942 = EDGE_LOOP ( 'NONE', ( #5116, #1457, #4424, #2078 ) ) ;
#5943 = FACE_OUTER_BOUND ( 'NONE', #3477, .T. ) ;
#5944 = AXIS2_PLACEMENT_3D ( 'NONE', #8584, #1965, #7971 ) ;
#5945 = DIRECTION ( 'NONE',  ( 0.000000000000000000, 0.000000000000000000, 1.000000000000000000 ) ) ;
#5946 = PRODUCT_RELATED_PRODUCT_CATEGORY ( 'part', '', ( #8034 ) ) ;
#5947 = CARTESIAN_POINT ( 'NONE',  ( 4.000000000000000888, 0.8228435280416209752, -3.430609588141487976 ) ) ;
#5948 = VECTOR ( 'NONE', #3857, 1000.000000000000000 ) ;
#5949 = DIRECTION ( 'NONE',  ( 0.000000000000000000, 0.000000000000000000, 1.000000000000000000 ) ) ;
#5950 = ORIENTED_EDGE ( 'NONE', *, *, #758, .T. ) ;
#5951 = SURFACE_SIDE_STYLE ('',( #4699 ) ) ;
#5952 = ORIENTED_EDGE ( 'NONE', *, *, #1276, .T. ) ;
#5953 = DIRECTION ( 'NONE',  ( 0.000000000000000000, 0.000000000000000000, 1.000000000000000000 ) ) ;
#5954 = VECTOR ( 'NONE', #8291, 1000.000000000000000 ) ;
#5955 = LINE ( 'NONE', #8027, #3294 ) ;
#5956 = DIRECTION ( 'NONE',  ( 0.000000000000000000, 0.000000000000000000, 1.000000000000000000 ) ) ;
#5957 = ORIENTED_EDGE ( 'NONE', *, *, #3938, .T. ) ;
#5958 = CARTESIAN_POINT ( 'NONE',  ( 93.00000000000000000, -4.999999999999998224, 140.0000000000000000 ) ) ;
#5959 = APPLICATION_CONTEXT ( 'automotive_design' ) ;
#5960 = CARTESIAN_POINT ( 'NONE',  ( 2.100000000000000089, 0.000000000000000000, -0.2800830152838844622 ) ) ;
#5961 = AXIS2_PLACEMENT_3D ( 'NONE', #3804, #7809, #8503 ) ;
#5962 = EDGE_CURVE ( 'NONE', #2893, #926, #8417, .T. ) ;
#5963 = DIRECTION ( 'NONE',  ( -0.000000000000000000, -0.000000000000000000, 1.000000000000000000 ) ) ;
#5964 = CARTESIAN_POINT ( 'NONE',  ( 10.00000000000000000, 0.000000000000000000, -27.99999999999999645 ) ) ;
#5965 = ADVANCED_FACE ( 'NONE', ( #421, #6992 ), #6949, .T. ) ;
#5966 = LINE ( 'NONE', #4665, #6977 ) ;
#5967 = ADVANCED_FACE ( 'NONE', ( #4990 ), #6336, .T. ) ;
#5968 = DIRECTION ( 'NONE',  ( -1.000000000000000000, 0.000000000000000000, -0.000000000000000000 ) ) ;
#5969 = EDGE_CURVE ( 'NONE', #7555, #4028, #8356, .T. ) ;
#5970 = CARTESIAN_POINT ( 'NONE',  ( 0.000000000000000000, 0.000000000000000000, -135.0000000000000000 ) ) ;
#5971 = SURFACE_SIDE_STYLE ('',( #5236 ) ) ;
#5972 = EDGE_LOOP ( 'NONE', ( #6816, #1744 ) ) ;
#5973 =( LENGTH_UNIT ( ) NAMED_UNIT ( * ) SI_UNIT ( .MILLI., .METRE. ) );
#5974 = EDGE_LOOP ( 'NONE', ( #7805, #1307 ) ) ;
#5975 = ORIENTED_EDGE ( 'NONE', *, *, #4473, .F. ) ;
#5976 = DIRECTION ( 'NONE',  ( 1.000000000000000000, -1.734723475976806848E-16, 0.000000000000000000 ) ) ;
#5977 = CARTESIAN_POINT ( 'NONE',  ( 88.00000000000000000, -20.00000000000000000, -121.8314250403154659 ) ) ;
#5978 = PLANE ( 'NONE',  #6051 ) ;
#5979 = VERTEX_POINT ( 'NONE', #2483 ) ;
#5980 = DIRECTION ( 'NONE',  ( 0.000000000000000000, 0.000000000000000000, 1.000000000000000000 ) ) ;
#5981 = CARTESIAN_POINT ( 'NONE',  ( 5.000000000000001776, -4.999999999999998224, 145.0000000000000284 ) ) ;
#5982 = DIRECTION ( 'NONE',  ( -3.100818213308542065E-17, -1.000000000000000000, 0.000000000000000000 ) ) ;
#5983 = PLANE ( 'NONE',  #4216 ) ;
#5984 = VERTEX_POINT ( 'NONE', #3081 ) ;
#5985 = VERTEX_POINT ( 'NONE', #5281 ) ;
#5986 = STYLED_ITEM ( 'NONE', ( #7804 ), #2539 ) ;
#5987 = CARTESIAN_POINT ( 'NONE',  ( 53.33333333333330017, -14.99999999999999822, 159.8500000000001080 ) ) ;
#5988 = CYLINDRICAL_SURFACE ( 'NONE', #7718, 10.00000000000000000 ) ;
#5989 = AXIS2_PLACEMENT_3D ( 'NONE', #4001, #8529, #5982 ) ;
#5990 = PRODUCT_DEFINITION_SHAPE ( 'NONE', 'NONE',  #8606 ) ;
#5991 = CARTESIAN_POINT ( 'NONE',  ( -4.999999999999998224, 135.0000000000000000, 15.00000000000000355 ) ) ;
#5992 = ORIENTED_EDGE ( 'NONE', *, *, #1593, .T. ) ;
#5993 =( GEOMETRIC_REPRESENTATION_CONTEXT ( 3 ) GLOBAL_UNCERTAINTY_ASSIGNED_CONTEXT ( ( #767 ) ) GLOBAL_UNIT_ASSIGNED_CONTEXT ( ( #3325, #2586, #4712 ) ) REPRESENTATION_CONTEXT ( 'NONE', 'WORKASPACE' ) );
#5994 = ADVANCED_FACE ( 'NONE', ( #7863 ), #7293, .F. ) ;
#5995 = EDGE_CURVE ( 'NONE', #1878, #7699, #8000, .T. ) ;
#5996 = ORIENTED_EDGE ( 'NONE', *, *, #8392, .T. ) ;
#5997 = CARTESIAN_POINT ( 'NONE',  ( 53.33333333333330017, -25.00000000000000000, 162.5000000000000853 ) ) ;
#5998 = EDGE_CURVE ( 'NONE', #4339, #5984, #10, .T. ) ;
#5999 = VECTOR ( 'NONE', #5953, 1000.000000000000000 ) ;
#6000 = VECTOR ( 'NONE', #3281, 1000.000000000000000 ) ;
#6001 = DIRECTION ( 'NONE',  ( 0.000000000000000000, 0.000000000000000000, 1.000000000000000000 ) ) ;
#6002 = CARTESIAN_POINT ( 'NONE',  ( 470.0000000000000000, 786.6649314574284517, 0.000000000000000000 ) ) ;
#6003 = ORIENTED_EDGE ( 'NONE', *, *, #1460, .F. ) ;
#6004 = CARTESIAN_POINT ( 'NONE',  ( 5.000000000000000000, 5.000000000000000000, -0.9999999999999940048 ) ) ;
#6005 = CIRCLE ( 'NONE', #5596, 10.00000000000000000 ) ;
#6006 = CARTESIAN_POINT ( 'NONE',  ( 53.33333333333330017, -20.00000000000000000, 159.8500000000001080 ) ) ;
#6007 = EDGE_CURVE ( 'NONE', #863, #1556, #7907, .T. ) ;
#6008 = CIRCLE ( 'NONE', #6438, 2.649999999999985700 ) ;
#6009 = VECTOR ( 'NONE', #6473, 1000.000000000000000 ) ;
#6010 = DIRECTION ( 'NONE',  ( 1.000000000000000000, 0.000000000000000000, 0.000000000000000000 ) ) ;
#6011 = DIRECTION ( 'NONE',  ( 0.000000000000000000, 0.000000000000000000, -1.000000000000000000 ) ) ;
#6012 = VECTOR ( 'NONE', #2474, 1000.000000000000000 ) ;
#6013 = CARTESIAN_POINT ( 'NONE',  ( 0.000000000000000000, 0.000000000000000000, -135.0000000000000000 ) ) ;
#6014 = DIRECTION ( 'NONE',  ( 0.000000000000000000, 0.000000000000000000, 1.000000000000000000 ) ) ;
#6015 = EDGE_LOOP ( 'NONE', ( #5198, #3830, #248 ) ) ;
#6016 = EDGE_LOOP ( 'NONE', ( #7862, #5027, #5044, #413 ) ) ;
#6017 = ORIENTED_EDGE ( 'NONE', *, *, #6909, .F. ) ;
#6018 = LINE ( 'NONE', #231, #4502 ) ;
#6019 = EDGE_CURVE ( 'NONE', #917, #1044, #398, .T. ) ;
#6020 = CARTESIAN_POINT ( 'NONE',  ( 219.9999999999999716, -15.00000000000000000, 159.8500000000001080 ) ) ;
#6021 = VECTOR ( 'NONE', #3200, 1000.000000000000000 ) ;
#6022 = ORIENTED_EDGE ( 'NONE', *, *, #5677, .F. ) ;
#6023 = DIRECTION ( 'NONE',  ( -1.000000000000000000, -0.000000000000000000, -0.000000000000000000 ) ) ;
#6024 = VERTEX_POINT ( 'NONE', #679 ) ;
#6025 = DIRECTION ( 'NONE',  ( 0.000000000000000000, -1.000000000000000000, 0.000000000000000000 ) ) ;
#6026 = AXIS2_PLACEMENT_3D ( 'NONE', #1606, #6115, #6819 ) ;
#6027 = DIRECTION ( 'NONE',  ( 0.000000000000000000, 0.000000000000000000, 1.000000000000000000 ) ) ;
#6028 = ADVANCED_FACE ( 'NONE', ( #6468 ), #5805, .T. ) ;
#6029 = DIRECTION ( 'NONE',  ( -0.6499189813095199719, 5.551115123125782702E-17, -0.7600034985008923272 ) ) ;
#6030 =( LENGTH_UNIT ( ) NAMED_UNIT ( * ) SI_UNIT ( .MILLI., .METRE. ) );
#6031 = ORIENTED_EDGE ( 'NONE', *, *, #5771, .T. ) ;
#6032 = ORIENTED_EDGE ( 'NONE', *, *, #8555, .T. ) ;
#6033 = CARTESIAN_POINT ( 'NONE',  ( 10.00000000000000000, 0.000000000000000000, -63.99999999999997158 ) ) ;
#6034 = EDGE_CURVE ( 'NONE', #765, #1337, #4378, .T. ) ;
#6035 = CARTESIAN_POINT ( 'NONE',  ( 5.000000000000000000, 5.000000000000000000, 140.0000000000000000 ) ) ;
#6036 = DIRECTION ( 'NONE',  ( -1.000000000000000000, 0.000000000000000000, 0.000000000000000000 ) ) ;
#6037 = PLANE ( 'NONE',  #3057 ) ;
#6038 = EDGE_LOOP ( 'NONE', ( #7601, #5588, #1037, #1098 ) ) ;
#6039 =( NAMED_UNIT ( * ) SI_UNIT ( $, .STERADIAN. ) SOLID_ANGLE_UNIT ( ) );
#6040 = DIRECTION ( 'NONE',  ( -1.000000000000000000, 0.000000000000000000, 0.000000000000000000 ) ) ;
#6041 = ORIENTED_EDGE ( 'NONE', *, *, #2025, .T. ) ;
#6042 = CARTESIAN_POINT ( 'NONE',  ( -5.000000000000000000, -5.000000000000000000, 34.00000000000000711 ) ) ;
#6043 = EDGE_CURVE ( 'NONE', #101, #5678, #1207, .T. ) ;
#6044 = ADVANCED_BREP_SHAPE_REPRESENTATION ( '', ( #2263, #594 ), #6566 ) ;
#6045 = AXIS2_PLACEMENT_3D ( 'NONE', #1520, #6951, #4827 ) ;
#6046 = PLANE ( 'NONE',  #2604 ) ;
#6047 = PLANE ( 'NONE',  #4977 ) ;
#6048 = ORIENTED_EDGE ( 'NONE', *, *, #6192, .F. ) ;
#6049 = CARTESIAN_POINT ( 'NONE',  ( 10.00000000000000000, 0.000000000000000000, 7.000000000000006217 ) ) ;
#6050 = CYLINDRICAL_SURFACE ( 'NONE', #23, 10.00000000000000000 ) ;
#6051 = AXIS2_PLACEMENT_3D ( 'NONE', #683, #7381, #1330 ) ;
#6052 = AXIS2_PLACEMENT_3D ( 'NONE', #6161, #6641, #8051 ) ;
#6053 = LINE ( 'NONE', #5535, #3510 ) ;
#6054 = CARTESIAN_POINT ( 'NONE',  ( 439.9999999999999432, -20.00000000000000000, 21.61857495968444454 ) ) ;
#6055 = COLOUR_RGB ( '',1.000000000000000000, 0.9490196078431372140, 0.9098039215686274384 ) ;
#6056 = DIRECTION ( 'NONE',  ( 0.000000000000000000, -1.000000000000000000, 0.000000000000000000 ) ) ;
#6057 = DIRECTION ( 'NONE',  ( -1.000000000000000000, 0.000000000000000000, 0.000000000000000000 ) ) ;
#6058 = AXIS2_PLACEMENT_3D ( 'NONE', #6656, #8073, #7981 ) ;
#6059 = EDGE_LOOP ( 'NONE', ( #5662, #1822, #5276 ) ) ;
#6060 = VERTEX_POINT ( 'NONE', #3251 ) ;
#6061 = UNCERTAINTY_MEASURE_WITH_UNIT (LENGTH_MEASURE( 1.000000000000000082E-05 ), #4534, 'distance_accuracy_value', 'NONE');
#6062 = VERTEX_POINT ( 'NONE', #5893 ) ;
#6063 = CYLINDRICAL_SURFACE ( 'NONE', #756, 10.00000000000000000 ) ;
#6064 = PRODUCT_DEFINITION_SHAPE ( 'NONE', 'NONE',  #8601 ) ;
#6065 = ORIENTED_EDGE ( 'NONE', *, *, #1931, .F. ) ;
#6066 = CARTESIAN_POINT ( 'NONE',  ( 0.000000000000000000, 0.000000000000000000, -0.9999999999999940048 ) ) ;
#6067 = ORIENTED_EDGE ( 'NONE', *, *, #7749, .F. ) ;
#6068 = LINE ( 'NONE', #904, #2824 ) ;
#6069 = PLANE ( 'NONE',  #3706 ) ;
#6070 = ITEM_DEFINED_TRANSFORMATION ( 'NONE', 'NONE', #2542,  #594 ) ;
#6071 = VERTEX_POINT ( 'NONE', #8481 ) ;
#6072 = VERTEX_POINT ( 'NONE', #6590 ) ;
#6073 = DIRECTION ( 'NONE',  ( 0.000000000000000000, 1.000000000000000000, 0.000000000000000000 ) ) ;
#6074 = CARTESIAN_POINT ( 'NONE',  ( 1.567478505476134606E-15, 4.618802153517012066, -3.433295621305382905 ) ) ;
#6075 = EDGE_CURVE ( 'NONE', #6478, #3075, #7949, .T. ) ;
#6076 = ADVANCED_FACE ( 'NONE', ( #5845 ), #4634, .F. ) ;
#6077 = DIRECTION ( 'NONE',  ( -0.000000000000000000, -0.000000000000000000, 1.000000000000000000 ) ) ;
#6078 = CARTESIAN_POINT ( 'NONE',  ( 2.449848172108560096, 3.432307619358740514, -3.503702292528905637 ) ) ;
#6079 = ORIENTED_EDGE ( 'NONE', *, *, #5183, .F. ) ;
#6080 = EDGE_CURVE ( 'NONE', #5816, #7885, #2648, .T. ) ;
#6081 = CARTESIAN_POINT ( 'NONE',  ( 5.000000000000000000, 5.000000000000000000, 148.0000000000000284 ) ) ;
#6082 = ORIENTED_EDGE ( 'NONE', *, *, #5724, .F. ) ;
#6083 = CARTESIAN_POINT ( 'NONE',  ( -5.000000000000001776, 5.000000000000001776, 148.0000000000000284 ) ) ;
#6084 = VECTOR ( 'NONE', #2665, 1000.000000000000000 ) ;
#6085 = DIRECTION ( 'NONE',  ( -0.000000000000000000, 1.000000000000000000, -0.000000000000000000 ) ) ;
#6086 = DIRECTION ( 'NONE',  ( -0.8191520442889902442, 0.000000000000000000, -0.5735764363510482688 ) ) ;
#6087 = VERTEX_POINT ( 'NONE', #5202 ) ;
#6088 = DIRECTION ( 'NONE',  ( 1.000000000000000000, 0.000000000000000000, 0.000000000000000000 ) ) ;
#6089 = EDGE_CURVE ( 'NONE', #4430, #6694, #8563, .T. ) ;
#6090 = CIRCLE ( 'NONE', #4851, 20.00000000000000000 ) ;
#6091 = CARTESIAN_POINT ( 'NONE',  ( -3.679171394226034675, -2.494631558665844739, -0.3503314178412558211 ) ) ;
#6092 = LINE ( 'NONE', #128, #1713 ) ;
#6093 = AXIS2_PLACEMENT_3D ( 'NONE', #4750, #6617, #6088 ) ;
#6094 = CYLINDRICAL_SURFACE ( 'NONE', #6250, 2.100000000000000089 ) ;
#6095 = CARTESIAN_POINT ( 'NONE',  ( 20.00000000000000000, 175.0000000000000284, 0.000000000000000000 ) ) ;
#6096 = DIRECTION ( 'NONE',  ( 0.000000000000000000, 0.000000000000000000, -1.000000000000000000 ) ) ;
#6097 = VERTEX_POINT ( 'NONE', #7825 ) ;
#6098 = ORIENTED_EDGE ( 'NONE', *, *, #7478, .T. ) ;
#6099 = EDGE_CURVE ( 'NONE', #8215, #5355, #1250, .T. ) ;
#6100 = ADVANCED_FACE ( 'NONE', ( #5241 ), #1947, .F. ) ;
#6101 = VERTEX_POINT ( 'NONE', #6633 ) ;
#6102 = FACE_OUTER_BOUND ( 'NONE', #4069, .T. ) ;
#6103 = EDGE_CURVE ( 'NONE', #8587, #7465, #3336, .T. ) ;
#6104 = PLANE ( 'NONE',  #2429 ) ;
#6105 = ORIENTED_EDGE ( 'NONE', *, *, #7281, .T. ) ;
#6106 = LINE ( 'NONE', #6859, #1616 ) ;
#6107 = EDGE_LOOP ( 'NONE', ( #330, #7221, #3874, #5680, #1378 ) ) ;
#6108 = DIRECTION ( 'NONE',  ( 0.000000000000000000, 0.000000000000000000, -1.000000000000000000 ) ) ;
#6109 = AXIS2_PLACEMENT_3D ( 'NONE', #635, #3291, #2640 ) ;
#6110 = DIRECTION ( 'NONE',  ( -1.000000000000000000, 1.734723475976807587E-16, 0.000000000000000000 ) ) ;
#6111 = CARTESIAN_POINT ( 'NONE',  ( -4.999999999999998224, -4.999999999999998224, 140.0000000000000000 ) ) ;
#6112 = ORIENTED_EDGE ( 'NONE', *, *, #3329, .T. ) ;
#6113 = ORIENTED_EDGE ( 'NONE', *, *, #2435, .F. ) ;
#6114 = DIRECTION ( 'NONE',  ( -1.000000000000000000, 0.000000000000000000, 0.000000000000000000 ) ) ;
#6115 = DIRECTION ( 'NONE',  ( 0.000000000000000000, 0.000000000000000000, -1.000000000000000000 ) ) ;
#6116 = EDGE_CURVE ( 'NONE', #6803, #5031, #8044, .T. ) ;
#6117 = LINE ( 'NONE', #4170, #3005 ) ;
#6118 = CARTESIAN_POINT ( 'NONE',  ( 5.000000000000000000, 5.000000000000000000, 140.0000000000000000 ) ) ;
#6119 = VERTEX_POINT ( 'NONE', #6804 ) ;
#6120 = LINE ( 'NONE', #157, #7055 ) ;
#6121 = DIRECTION ( 'NONE',  ( 0.000000000000000000, 0.000000000000000000, 1.000000000000000000 ) ) ;
#6122 = FACE_OUTER_BOUND ( 'NONE', #565, .T. ) ;
#6123 = EDGE_LOOP ( 'NONE', ( #4182, #2994, #5039, #8091 ) ) ;
#6124 = CARTESIAN_POINT ( 'NONE',  ( 2.500000000000000000, 2.357898499370433054, -1.951563910473907981E-15 ) ) ;
#6125 = DIRECTION ( 'NONE',  ( -0.000000000000000000, -0.000000000000000000, 1.000000000000000000 ) ) ;
#6126 = ADVANCED_FACE ( 'NONE', ( #1503 ), #6063, .T. ) ;
#6127 =( REPRESENTATION_RELATIONSHIP ('NONE','NONE', #3312, #4754 ) REPRESENTATION_RELATIONSHIP_WITH_TRANSFORMATION ( #1368 )SHAPE_REPRESENTATION_RELATIONSHIP( ) );
#6128 = EDGE_CURVE ( 'NONE', #2389, #4446, #7377, .T. ) ;
#6129 = PRODUCT_DEFINITION_FORMATION_WITH_SPECIFIED_SOURCE ( 'ANY', '', #3920, .NOT_KNOWN. ) ;
#6130 = MECHANICAL_DESIGN_GEOMETRIC_PRESENTATION_REPRESENTATION (  '', ( #2543 ), #3644 ) ;
#6131 = CARTESIAN_POINT ( 'NONE',  ( 386.6666666666666288, -14.99999999999999822, 159.8500000000001080 ) ) ;
#6132 = DIRECTION ( 'NONE',  ( 0.000000000000000000, 0.000000000000000000, 1.000000000000000000 ) ) ;
#6133 = EDGE_LOOP ( 'NONE', ( #7737, #2516, #7917, #5249 ) ) ;
#6134 = FACE_BOUND ( 'NONE', #3468, .T. ) ;
#6135 = PRODUCT_DEFINITION_SHAPE ( 'NONE', 'NONE',  #2614 ) ;
#6136 = PLANE ( 'NONE',  #1854 ) ;
#6137 = AXIS2_PLACEMENT_3D ( 'NONE', #7680, #1140, #3149 ) ;
#6138 = B_SPLINE_CURVE_WITH_KNOTS ( 'NONE', 3,
 ( #3999, #8487, #2569, #1956 ),
 .UNSPECIFIED., .F., .F.,
 ( 4, 4 ),
 ( 0.000000000000000000, 0.002452478801916361129 ),
 .UNSPECIFIED. ) ;
#6139 = CARTESIAN_POINT ( 'NONE',  ( 0.000000000000000000, 0.000000000000000000, 34.00000000000000711 ) ) ;
#6140 = VECTOR ( 'NONE', #5481, 1000.000000000000000 ) ;
#6141 = VECTOR ( 'NONE', #4782, 1000.000000000000000 ) ;
#6142 = LINE ( 'NONE', #7545, #6945 ) ;
#6143 = AXIS2_PLACEMENT_3D ( 'NONE', #219, #2973, #2236 ) ;
#6144 = CARTESIAN_POINT ( 'NONE',  ( 2.344047193898588954, 3.265465875126468021, -5.031375706690542042E-16 ) ) ;
#6145 = FACE_OUTER_BOUND ( 'NONE', #7475, .T. ) ;
#6146 = ORIENTED_EDGE ( 'NONE', *, *, #6880, .F. ) ;
#6147 = AXIS2_PLACEMENT_3D ( 'NONE', #515, #3174, #6514 ) ;
#6148 = EDGE_LOOP ( 'NONE', ( #870, #5582, #552, #2108, #7629, #6864 ) ) ;
#6149 = EDGE_LOOP ( 'NONE', ( #4972, #8281, #228, #4080 ) ) ;
#6150 = DIRECTION ( 'NONE',  ( -0.000000000000000000, -0.000000000000000000, 1.000000000000000000 ) ) ;
#6151 = VECTOR ( 'NONE', #733, 1000.000000000000000 ) ;
#6152 = SURFACE_SIDE_STYLE ('',( #5458 ) ) ;
#6153 = AXIS2_PLACEMENT_3D ( 'NONE', #6255, #6734, #8186 ) ;
#6154 = MECHANICAL_DESIGN_GEOMETRIC_PRESENTATION_REPRESENTATION (  '', ( #7139 ), #177 ) ;
#6155 = ADVANCED_FACE ( 'NONE', ( #7338 ), #5056, .F. ) ;
#6156 = ADVANCED_FACE ( 'NONE', ( #2806 ), #3814, .T. ) ;
#6157 = VERTEX_POINT ( 'NONE', #4073 ) ;
#6158 = CARTESIAN_POINT ( 'NONE',  ( 5.000000000000000000, 5.000000000000000000, 34.00000000000000711 ) ) ;
#6159 = ORIENTED_EDGE ( 'NONE', *, *, #7490, .F. ) ;
#6160 = DIRECTION ( 'NONE',  ( 0.000000000000000000, 0.000000000000000000, 1.000000000000000000 ) ) ;
#6161 = CARTESIAN_POINT ( 'NONE',  ( 0.000000000000000000, 0.000000000000000000, 3.469446951953614189E-15 ) ) ;
#6162 = CONTEXT_DEPENDENT_SHAPE_REPRESENTATION ( #3032, #3363 ) ;
#6163 = EDGE_LOOP ( 'NONE', ( #6377, #2538, #633, #5211 ) ) ;
#6164 = EDGE_LOOP ( 'NONE', ( #2970, #1500, #323, #184 ) ) ;
#6165 = CIRCLE ( 'NONE', #2144, 10.00000000000000000 ) ;
#6166 = CARTESIAN_POINT ( 'NONE',  ( 0.000000000000000000, 0.000000000000000000, 27.00000000000000711 ) ) ;
#6167 = CARTESIAN_POINT ( 'NONE',  ( 82.99999999999998579, 5.000000000000001776, 145.0000000000000284 ) ) ;
#6168 = AXIS2_PLACEMENT_3D ( 'NONE', #4045, #734, #4006 ) ;
#6169 = CARTESIAN_POINT ( 'NONE',  ( -4.999999999999998224, -4.999999999999998224, 145.0000000000000284 ) ) ;
#6170 = DIRECTION ( 'NONE',  ( 0.000000000000000000, 1.000000000000000000, 0.000000000000000000 ) ) ;
#6171 = ADVANCED_FACE ( 'NONE', ( #3378 ), #852, .F. ) ;
#6172 = EDGE_LOOP ( 'NONE', ( #962, #3668, #8221, #1150 ) ) ;
#6173 = DIRECTION ( 'NONE',  ( 0.000000000000000000, 0.000000000000000000, 1.000000000000000000 ) ) ;
#6174 = CARTESIAN_POINT ( 'NONE',  ( -5.000000000000000000, -5.000000000000000000, -0.9999999999999940048 ) ) ;
#6175 = ORIENTED_EDGE ( 'NONE', *, *, #7731, .T. ) ;
#6176 = ORIENTED_EDGE ( 'NONE', *, *, #2468, .F. ) ;
#6177 = PLANE ( 'NONE',  #7546 ) ;
#6178 = CARTESIAN_POINT ( 'NONE',  ( 347.0000000000000000, -4.999999999999998224, 145.0000000000000284 ) ) ;
#6179 = CARTESIAN_POINT ( 'NONE',  ( -5.000000000000000000, -5.000000000000000000, 148.0000000000000284 ) ) ;
#6180 = DIRECTION ( 'NONE',  ( -0.000000000000000000, -0.000000000000000000, 1.000000000000000000 ) ) ;
#6181 = VERTEX_POINT ( 'NONE', #6718 ) ;
#6182 = CARTESIAN_POINT ( 'NONE',  ( 2.500000000000000000, -1.178949249685213863, 2.042000000000002924 ) ) ;
#6183 = FILL_AREA_STYLE ('',( #262 ) ) ;
#6184 = FACE_OUTER_BOUND ( 'NONE', #3028, .T. ) ;
#6185 = LINE ( 'NONE', #7542, #4342 ) ;
#6186 = VECTOR ( 'NONE', #4785, 1000.000000000000000 ) ;
#6187 = EDGE_CURVE ( 'NONE', #1781, #5500, #6165, .T. ) ;
#6188 = DIRECTION ( 'NONE',  ( -1.734723475976807587E-16, 1.000000000000000000, 0.000000000000000000 ) ) ;
#6189 = CARTESIAN_POINT ( 'NONE',  ( 444.9999999999999432, 5.000000000000000000, 139.9990000000000236 ) ) ;
#6190 = CARTESIAN_POINT ( 'NONE',  ( 176.0000000000000000, -25.00000000000000000, -86.63142504031547730 ) ) ;
#6191 = ORIENTED_EDGE ( 'NONE', *, *, #6430, .T. ) ;
#6192 = EDGE_CURVE ( 'NONE', #7614, #1399, #3506, .T. ) ;
#6193 = AXIS2_PLACEMENT_3D ( 'NONE', #6637, #6594, #4593 ) ;
#6194 = EDGE_LOOP ( 'NONE', ( #4985, #8558, #5119 ) ) ;
#6195 = CLOSED_SHELL ( 'NONE', ( #2924, #3562, #4781, #2216, #6530, #4431, #548, #2262, #2921, #2720, #3942, #8143, #2684, #5253, #7766, #7950, #7583, #1872, #4839, #6938 ) ) ;
#6196 = CARTESIAN_POINT ( 'NONE',  ( 10.00000000000000000, 0.000000000000000000, -27.99999999999999645 ) ) ;
#6197 = CARTESIAN_POINT ( 'NONE',  ( 176.0000000000000000, -20.00000000000000000, -86.63142504031547730 ) ) ;
#6198 = PRESENTATION_STYLE_ASSIGNMENT (( #6855 ) ) ;
#6199 = VECTOR ( 'NONE', #2392, 1000.000000000000000 ) ;
#6200 =( BOUNDED_SURFACE ( )  B_SPLINE_SURFACE ( 3, 2, ( 
 ( #1350, #4011, #1396 ),
 ( #4050, #2184, #7445 ),
 ( #6222, #4267, #2275 ),
 ( #5524, #4921, #6916 ),
 ( #2876, #6875, #7532 ),
 ( #1613, #7581, #4178 ) ),
 .UNSPECIFIED., .F., .F., .T. ) 
 B_SPLINE_SURFACE_WITH_KNOTS ( ( 4, 2, 4 ),
 ( 3, 3 ),
 ( 0.02032853247518125531, 0.02278863295364820865, 0.02524873343211516200 ),
 ( 0.000000000000000000, 1.000000000000000000 ),
 .UNSPECIFIED. ) 
 GEOMETRIC_REPRESENTATION_ITEM ( )  RATIONAL_B_SPLINE_SURFACE ( (
 ( 1.000000000000000000, 0.8047781615896836271, 1.000000000000000000),
 ( 1.000000000000000000, 0.8123767586289967202, 1.000000000000000000),
 ( 1.000000000000000000, 0.8190662415563443322, 1.000000000000000000),
 ( 1.000000000000000000, 0.8192361015669982205, 1.000000000000000000),
 ( 1.000000000000000000, 0.8126135807103181952, 1.000000000000000000),
 ( 1.000000000000000000, 0.8047712338318587788, 1.000000000000000000) ) ) 
 REPRESENTATION_ITEM ( '' )  SURFACE ( )  );
#6201 = ORIENTED_EDGE ( 'NONE', *, *, #899, .F. ) ;
#6202 = CARTESIAN_POINT ( 'NONE',  ( 2.500000000000000000, 2.357898499370433054, -1.951563910473907981E-15 ) ) ;
#6203 = ORIENTED_EDGE ( 'NONE', *, *, #3534, .T. ) ;
#6204 = LINE ( 'NONE', #5549, #3384 ) ;
#6205 = DIRECTION ( 'NONE',  ( 0.000000000000000000, -1.000000000000000000, 0.000000000000000000 ) ) ;
#6206 = ITEM_DEFINED_TRANSFORMATION ( 'NONE', 'NONE', #5432,  #594 ) ;
#6207 = DIRECTION ( 'NONE',  ( -1.000000000000000000, 0.000000000000000000, -0.000000000000000000 ) ) ;
#6208 = ORIENTED_EDGE ( 'NONE', *, *, #1261, .T. ) ;
#6209 = ORIENTED_EDGE ( 'NONE', *, *, #7639, .T. ) ;
#6210 = EDGE_CURVE ( 'NONE', #819, #6781, #5502, .T. ) ;
#6212 = AXIS2_PLACEMENT_3D ( 'NONE', #2753, #6699, #660 ) ;
#6211 = CARTESIAN_POINT ( 'NONE',  ( 0.000000000000000000, 1.178949249685218525, 2.041999999999999371 ) ) ;
#6213 = DIRECTION ( 'NONE',  ( 0.000000000000000000, 0.000000000000000000, 1.000000000000000000 ) ) ;
#6214 = EDGE_CURVE ( 'NONE', #3178, #3270, #6018, .T. ) ;
#6215 = LINE ( 'NONE', #4217, #5080 ) ;
#6216 = CARTESIAN_POINT ( 'NONE',  ( 4.236525694536557474, -2.416953475386482530, -3.751298745799839462 ) ) ;
#6217 = ORIENTED_EDGE ( 'NONE', *, *, #3056, .T. ) ;
#6218 = SHAPE_REPRESENTATION_RELATIONSHIP ( 'NONE' , 'NONE' ,  #4706, #5415 ) ;
#6219 = DIRECTION ( 'NONE',  ( 1.000000000000000000, 0.000000000000000000, -0.000000000000000000 ) ) ;
#6220 = ORIENTED_EDGE ( 'NONE', *, *, #7528, .F. ) ;
#6221 = VERTEX_POINT ( 'NONE', #187 ) ;
#6222 = CARTESIAN_POINT ( 'NONE',  ( -1.243802165048909503, 3.900692638707381921, -3.223146290109805800 ) ) ;
#6223 = CARTESIAN_POINT ( 'NONE',  ( -10.00000000000000000, 1.224646799147353256E-15, -63.99999999999997158 ) ) ;
#6224 = CARTESIAN_POINT ( 'NONE',  ( 2.500000000000000000, 1.178949249685213863, -2.042000000000001148 ) ) ;
#6225 = CARTESIAN_POINT ( 'NONE',  ( -5.000000000000000000, -5.000000000000000000, 148.0000000000000284 ) ) ;
#6226 = ORIENTED_EDGE ( 'NONE', *, *, #3382, .F. ) ;
#6227 = FACE_BOUND ( 'NONE', #4004, .T. ) ;
#6228 =( NAMED_UNIT ( * ) SI_UNIT ( $, .STERADIAN. ) SOLID_ANGLE_UNIT ( ) );
#6229 = LINE ( 'NONE', #264, #6427 ) ;
#6230 = AXIS2_PLACEMENT_3D ( 'NONE', #5787, #3707, #8460 ) ;
#6231 = FACE_OUTER_BOUND ( 'NONE', #52, .T. ) ;
#6232 = FACE_OUTER_BOUND ( 'NONE', #6107, .T. ) ;
#6233 = EDGE_CURVE ( 'NONE', #6369, #3976, #5749, .T. ) ;
#6234 = FACE_OUTER_BOUND ( 'NONE', #6247, .T. ) ;
#6235 = DIRECTION ( 'NONE',  ( -0.000000000000000000, -0.000000000000000000, 1.000000000000000000 ) ) ;
#6236 = CIRCLE ( 'NONE', #826, 0.2000000000000000944 ) ;
#6237 = ORIENTED_EDGE ( 'NONE', *, *, #2741, .F. ) ;
#6238 = EDGE_LOOP ( 'NONE', ( #270, #6314, #8233, #2331, #7482 ) ) ;
#6239 = EDGE_CURVE ( 'NONE', #243, #5734, #5413, .T. ) ;
#6240 = ORIENTED_EDGE ( 'NONE', *, *, #88, .T. ) ;
#6241 = PLANE ( 'NONE',  #5608 ) ;
#6242 = EDGE_CURVE ( 'NONE', #2989, #3079, #4636, .T. ) ;
#6243 = VECTOR ( 'NONE', #2330, 1000.000000000000000 ) ;
#6244 = EDGE_CURVE ( 'NONE', #7506, #6477, #3670, .T. ) ;
#6245 = ORIENTED_EDGE ( 'NONE', *, *, #2534, .F. ) ;
#6246 = CARTESIAN_POINT ( 'NONE',  ( -5.000000000000000000, -5.000000000000000000, -36.00000000000000000 ) ) ;
#6247 = EDGE_LOOP ( 'NONE', ( #2789, #5340, #3132, #2476 ) ) ;
#6248 =( LENGTH_UNIT ( ) NAMED_UNIT ( * ) SI_UNIT ( .MILLI., .METRE. ) );
#6249 = LINE ( 'NONE', #5681, #4402 ) ;
#6250 = AXIS2_PLACEMENT_3D ( 'NONE', #5319, #3983, #6664 ) ;
#6251 = EDGE_LOOP ( 'NONE', ( #4230, #6041, #4937, #6947 ) ) ;
#6252 = ORIENTED_EDGE ( 'NONE', *, *, #5388, .T. ) ;
#6253 = CARTESIAN_POINT ( 'NONE',  ( -4.198928548860774157, 0.8158838809860065044, -3.526471437616918170 ) ) ;
#6254 = ADVANCED_BREP_SHAPE_REPRESENTATION ( '', ( #2244, #594 ), #6685 ) ;
#6255 = CARTESIAN_POINT ( 'NONE',  ( 303.3333333333333144, -15.00000000000000000, 162.5000000000000853 ) ) ;
#6256 = PLANE ( 'NONE',  #8566 ) ;
#6257 = CARTESIAN_POINT ( 'NONE',  ( 2.725741868436127202, -3.045094352033990148, -3.220599429844051453 ) ) ;
#6258 = EDGE_LOOP ( 'NONE', ( #4125, #1801, #7860, #4762 ) ) ;
#6259 = CARTESIAN_POINT ( 'NONE',  ( 0.000000000000000000, 0.000000000000000000, 0.000000000000000000 ) ) ;
#6260 = PLANE ( 'NONE',  #1120 ) ;
#6261 = VERTEX_POINT ( 'NONE', #3464 ) ;
#6262 = VERTEX_POINT ( 'NONE', #8172 ) ;
#6263 = CYLINDRICAL_SURFACE ( 'NONE', #2683, 10.00000000000000000 ) ;
#6264 = LINE ( 'NONE', #2964, #5883 ) ;
#6265 = CARTESIAN_POINT ( 'NONE',  ( 10.00000000000000000, 0.000000000000000000, 7.000000000000006217 ) ) ;
#6266 = ADVANCED_FACE ( 'NONE', ( #6102 ), #3549, .F. ) ;
#6267 = DIRECTION ( 'NONE',  ( -0.000000000000000000, -0.000000000000000000, 1.000000000000000000 ) ) ;
#6268 = VERTEX_POINT ( 'NONE', #4030 ) ;
#6269 = ADVANCED_FACE ( 'NONE', ( #6673 ), #4721, .F. ) ;
#6270 = FACE_BOUND ( 'NONE', #6762, .T. ) ;
#6271 = EDGE_CURVE ( 'NONE', #1828, #6087, #1876, .T. ) ;
#6272 = CARTESIAN_POINT ( 'NONE',  ( -4.000000000000000000, -2.309401076758515803, -0.4999999999999995559 ) ) ;
#6273 = PRESENTATION_LAYER_ASSIGNMENT (  '', '', ( #3777 ) ) ;
#6274 = FACE_OUTER_BOUND ( 'NONE', #2959, .T. ) ;
#6275 = CARTESIAN_POINT ( 'NONE',  ( 2.500000000000000000, 0.000000000000000000, 0.000000000000000000 ) ) ;
#6276 = CARTESIAN_POINT ( 'NONE',  ( -2.742827927723112236, -3.035229711105190464, -3.433252694550595230 ) ) ;
#6277 = PRESENTATION_STYLE_ASSIGNMENT (( #3625 ) ) ;
#6278 = AXIS2_PLACEMENT_3D ( 'NONE', #5338, #6680, #7915 ) ;
#6280 = ORIENTED_EDGE ( 'NONE', *, *, #7991, .F. ) ;
#6279 = EDGE_CURVE ( 'NONE', #8107, #1399, #1030, .T. ) ;
#6281 = VECTOR ( 'NONE', #4063, 1000.000000000000000 ) ;
#6282 = ORIENTED_EDGE ( 'NONE', *, *, #681, .F. ) ;
#6283 = EDGE_LOOP ( 'NONE', ( #1139, #5217, #8366, #3164 ) ) ;
#6284 = CIRCLE ( 'NONE', #587, 2.649999999999985700 ) ;
#6285 = DIRECTION ( 'NONE',  ( 0.000000000000000000, 0.000000000000000000, -1.000000000000000000 ) ) ;
#6286 = DIRECTION ( 'NONE',  ( 0.000000000000000000, 1.000000000000000000, 0.000000000000000000 ) ) ;
#6287 = AXIS2_PLACEMENT_3D ( 'NONE', #6885, #4798, #6968 ) ;
#6288 = ORIENTED_EDGE ( 'NONE', *, *, #6908, .T. ) ;
#6289 = FACE_OUTER_BOUND ( 'NONE', #689, .T. ) ;
#6290 = VECTOR ( 'NONE', #1997, 1000.000000000000000 ) ;
#6291 = ORIENTED_EDGE ( 'NONE', *, *, #442, .T. ) ;
#6292 = DIRECTION ( 'NONE',  ( 0.000000000000000000, 0.000000000000000000, 1.000000000000000000 ) ) ;
#6293 = CONTEXT_DEPENDENT_SHAPE_REPRESENTATION ( #3308, #1788 ) ;
#6294 = ORIENTED_EDGE ( 'NONE', *, *, #7443, .T. ) ;
#6295 = AXIS2_PLACEMENT_3D ( 'NONE', #7931, #7269, #79 ) ;
#6296 = ORIENTED_EDGE ( 'NONE', *, *, #2955, .T. ) ;
#6297 = CYLINDRICAL_SURFACE ( 'NONE', #211, 10.00000000000000000 ) ;
#6298 = LINE ( 'NONE', #2355, #5742 ) ;
#6299 =( REPRESENTATION_RELATIONSHIP ('NONE','NONE', #3312, #1479 ) REPRESENTATION_RELATIONSHIP_WITH_TRANSFORMATION ( #4778 )SHAPE_REPRESENTATION_RELATIONSHIP( ) );
#6300 = FACE_OUTER_BOUND ( 'NONE', #1526, .T. ) ;
#6301 = CARTESIAN_POINT ( 'NONE',  ( 4.101954839143060028, 2.368264730582927857, -3.681130640444267854 ) ) ;
#6302 = ORIENTED_EDGE ( 'NONE', *, *, #4793, .T. ) ;
#6303 = CIRCLE ( 'NONE', #5614, 2.649999999999985700 ) ;
#6304 = CARTESIAN_POINT ( 'NONE',  ( 88.00000000000000000, -20.00000000000000000, 35.66857495968456249 ) ) ;
#6305 = DIRECTION ( 'NONE',  ( -1.000000000000000000, 0.000000000000000000, 0.000000000000000000 ) ) ;
#6306 = ORIENTED_EDGE ( 'NONE', *, *, #6376, .F. ) ;
#6307 = ADVANCED_FACE ( 'NONE', ( #320 ), #6241, .F. ) ;
#6308 = ORIENTED_EDGE ( 'NONE', *, *, #2791, .F. ) ;
#6309 = DIRECTION ( 'NONE',  ( 0.000000000000000000, 0.000000000000000000, -1.000000000000000000 ) ) ;
#6310 = LINE ( 'NONE', #7090, #3678 ) ;
#6311 = VECTOR ( 'NONE', #6125, 1000.000000000000000 ) ;
#6312 = CARTESIAN_POINT ( 'NONE',  ( 5.000000000000000000, -5.000000000000000000, 148.0000000000000284 ) ) ;
#6313 = DIRECTION ( 'NONE',  ( -1.000000000000000000, 0.000000000000000000, -0.000000000000000000 ) ) ;
#6314 = ORIENTED_EDGE ( 'NONE', *, *, #5204, .T. ) ;
#6315 = CARTESIAN_POINT ( 'NONE',  ( -5.000000000000000000, -5.000000000000000000, 148.0000000000000284 ) ) ;
#6316 = EDGE_LOOP ( 'NONE', ( #1634, #3548, #2834, #5560 ) ) ;
#6317 = CARTESIAN_POINT ( 'NONE',  ( 20.00000000000000000, 135.0000000000000000, 40.00000000000000000 ) ) ;
#6318 = AXIS2_PLACEMENT_3D ( 'NONE', #6508, #3210, #4508 ) ;
#6319 = EDGE_CURVE ( 'NONE', #4430, #5788, #7602, .T. ) ;
#6320 = DIRECTION ( 'NONE',  ( -1.000000000000000000, 0.000000000000000000, -0.000000000000000000 ) ) ;
#6321 = DIRECTION ( 'NONE',  ( -0.000000000000000000, -0.000000000000000000, 1.000000000000000000 ) ) ;
#6322 = DIRECTION ( 'NONE',  ( 1.000000000000000000, 0.000000000000000000, 0.000000000000000000 ) ) ;
#6323 = CARTESIAN_POINT ( 'NONE',  ( -3.999999999998910649, -1.658469974638591804, -3.531532913075256186 ) ) ;
#6324 = ORIENTED_EDGE ( 'NONE', *, *, #8567, .T. ) ;
#6325 = ORIENTED_EDGE ( 'NONE', *, *, #6383, .T. ) ;
#6326 = CARTESIAN_POINT ( 'NONE',  ( 2.345747346278113987, -3.264484291692503870, -0.01223254789874484924 ) ) ;
#6327 = CARTESIAN_POINT ( 'NONE',  ( 219.9999999999999716, -25.00000000000000000, 159.8500000000001080 ) ) ;
#6328 = CARTESIAN_POINT ( 'NONE',  ( 20.00000000000000000, 0.000000000000000000, -191.5685424949238325 ) ) ;
#6329 = EDGE_LOOP ( 'NONE', ( #5301, #2461 ) ) ;
#6330 = AXIS2_PLACEMENT_3D ( 'NONE', #2577, #1797, #433 ) ;
#6331 = DIRECTION ( 'NONE',  ( -0.000000000000000000, 1.000000000000000000, -0.000000000000000000 ) ) ;
#6332 = ORIENTED_EDGE ( 'NONE', *, *, #6719, .F. ) ;
#6333 = DIRECTION ( 'NONE',  ( 1.000000000000000000, -1.734723475976806848E-16, 0.000000000000000000 ) ) ;
#6334 = ORIENTED_EDGE ( 'NONE', *, *, #1790, .F. ) ;
#6335 = VERTEX_POINT ( 'NONE', #6935 ) ;
#6336 = CYLINDRICAL_SURFACE ( 'NONE', #5894, 2.500000000000000888 ) ;
#6337 = DIRECTION ( 'NONE',  ( -0.000000000000000000, 1.000000000000000000, -0.000000000000000000 ) ) ;
#6338 = AXIS2_PLACEMENT_3D ( 'NONE', #2940, #6724, #6899 ) ;
#6339 = VECTOR ( 'NONE', #859, 1000.000000000000000 ) ;
#6340 = CARTESIAN_POINT ( 'NONE',  ( -5.000000000000000000, -5.000000000000000000, -63.99999999999997158 ) ) ;
#6341 = CARTESIAN_POINT ( 'NONE',  ( 5.000000000000001776, 140.0000000000000000, 15.00000000000000355 ) ) ;
#6342 = EDGE_LOOP ( 'NONE', ( #7935, #7014 ) ) ;
#6343 = VECTOR ( 'NONE', #1397, 1000.000000000000000 ) ;
#6344 = DIRECTION ( 'NONE',  ( 6.123233995736766036E-17, -1.000000000000000000, 0.000000000000000000 ) ) ;
#6345 = PLANE ( 'NONE',  #7369 ) ;
#6346 = EDGE_LOOP ( 'NONE', ( #8404, #305, #5303, #7310, #8083 ) ) ;
#6347 = ORIENTED_EDGE ( 'NONE', *, *, #11, .F. ) ;
#6348 = EDGE_CURVE ( 'NONE', #808, #1995, #1726, .T. ) ;
#6349 = LINE ( 'NONE', #3093, #4354 ) ;
#6350 = CARTESIAN_POINT ( 'NONE',  ( 386.6666666666666288, -25.00000000000000000, 159.8500000000001080 ) ) ;
#6351 = ADVANCED_FACE ( 'NONE', ( #3072, #4983 ), #4329, .T. ) ;
#6352 = B_SPLINE_CURVE_WITH_KNOTS ( 'NONE', 3,
 ( #782, #4783, #866, #8275, #3437, #6074 ),
 .UNSPECIFIED., .F., .F.,
 ( 4, 2, 4 ),
 ( -3.640115492407174633E-06, 0.0002066546034006553863, 0.0004169493222937179812 ),
 .UNSPECIFIED. ) ;
#6353 = ADVANCED_FACE ( 'NONE', ( #4417 ), #8345, .T. ) ;
#6354 = DIRECTION ( 'NONE',  ( 0.000000000000000000, 0.000000000000000000, -1.000000000000000000 ) ) ;
#6355 = FACE_OUTER_BOUND ( 'NONE', #4316, .T. ) ;
#6356 = ORIENTED_EDGE ( 'NONE', *, *, #5161, .F. ) ;
#6357 = FACE_OUTER_BOUND ( 'NONE', #1509, .T. ) ;
#6358 = FILL_AREA_STYLE_COLOUR ( '', #2246 ) ;
#6359 = ORIENTED_EDGE ( 'NONE', *, *, #1740, .T. ) ;
#6360 = CARTESIAN_POINT ( 'NONE',  ( 0.5449313310647804220, 4.304185902836899835, -3.316620875263383894 ) ) ;
#6361 = CARTESIAN_POINT ( 'NONE',  ( -20.00000000000000000, 2.449293598294706513E-15, -14.56854249492377207 ) ) ;
#6362 = CARTESIAN_POINT ( 'NONE',  ( -10.00000000000000000, 1.224646799147353059E-15, -27.99999999999999645 ) ) ;
#6363 = CARTESIAN_POINT ( 'NONE',  ( 434.9999999999999432, -4.999999999999998224, 145.0000000000000284 ) ) ;
#6364 = LINE ( 'NONE', #1851, #1243 ) ;
#6365 = DIRECTION ( 'NONE',  ( 0.000000000000000000, 0.000000000000000000, 1.000000000000000000 ) ) ;
#6366 = EDGE_CURVE ( 'NONE', #6900, #5850, #2386, .T. ) ;
#6367 = EDGE_LOOP ( 'NONE', ( #6282, #4506, #3017, #861 ) ) ;
#6368 = VECTOR ( 'NONE', #3098, 1000.000000000000000 ) ;
#6369 = VERTEX_POINT ( 'NONE', #6413 ) ;
#6370 = CARTESIAN_POINT ( 'NONE',  ( 0.000000000000000000, 0.000000000000000000, -97.99999999999997158 ) ) ;
#6371 = CARTESIAN_POINT ( 'NONE',  ( -5.000000000000001776, 5.000000000000001776, 140.0000000000000000 ) ) ;
#6372 = UNCERTAINTY_MEASURE_WITH_UNIT (LENGTH_MEASURE( 1.000000000000000082E-05 ), #657, 'distance_accuracy_value', 'NONE');
#6373 = VECTOR ( 'NONE', #5926, 1000.000000000000000 ) ;
#6374 = ORIENTED_EDGE ( 'NONE', *, *, #3565, .T. ) ;
#6375 = CARTESIAN_POINT ( 'NONE',  ( -10.00000000000000000, 1.224646799147353256E-15, -97.99999999999997158 ) ) ;
#6376 = EDGE_CURVE ( 'NONE', #5766, #1828, #3593, .T. ) ;
#6377 = ORIENTED_EDGE ( 'NONE', *, *, #2295, .F. ) ;
#6378 = ADVANCED_FACE ( 'NONE', ( #7691 ), #4287, .F. ) ;
#6379 =( NAMED_UNIT ( * ) SI_UNIT ( $, .STERADIAN. ) SOLID_ANGLE_UNIT ( ) );
#6380 = DIRECTION ( 'NONE',  ( -1.000000000000000000, 1.734723475976806848E-16, -0.000000000000000000 ) ) ;
#6381 = ITEM_DEFINED_TRANSFORMATION ( 'NONE', 'NONE', #5165,  #594 ) ;
#6382 = ORIENTED_EDGE ( 'NONE', *, *, #7315, .T. ) ;
#6383 = EDGE_CURVE ( 'NONE', #3347, #5639, #273, .T. ) ;
#6384 = ORIENTED_EDGE ( 'NONE', *, *, #666, .F. ) ;
#6385 = DIRECTION ( 'NONE',  ( 0.000000000000000000, 0.000000000000000000, -1.000000000000000000 ) ) ;
#6386 = CIRCLE ( 'NONE', #7358, 2.649999999999985700 ) ;
#6387 = DIRECTION ( 'NONE',  ( 1.000000000000000000, 0.000000000000000000, 0.000000000000000000 ) ) ;
#6388 = DIRECTION ( 'NONE',  ( 1.000000000000000000, 0.000000000000000000, 0.000000000000000000 ) ) ;
#6389 = VECTOR ( 'NONE', #4017, 1000.000000000000000 ) ;
#6390 = EDGE_LOOP ( 'NONE', ( #4165, #3969, #1175, #3826 ) ) ;
#6391 = DIRECTION ( 'NONE',  ( 6.123233985217515406E-17, -1.000000000000000000, -2.214089701702311143E-25 ) ) ;
#6392 = DIRECTION ( 'NONE',  ( 0.000000000000000000, 0.000000000000000000, 1.000000000000000000 ) ) ;
#6393 = EDGE_LOOP ( 'NONE', ( #1074, #2912, #1483 ) ) ;
#6394 = ORIENTED_EDGE ( 'NONE', *, *, #1168, .T. ) ;
#6395 = DIRECTION ( 'NONE',  ( 1.000000000000000000, -1.734723475976806848E-16, 0.000000000000000000 ) ) ;
#6396 = CARTESIAN_POINT ( 'NONE',  ( 20.00000000000000000, 140.0000000000000000, 40.00000000000000000 ) ) ;
#6397 = AXIS2_PLACEMENT_3D ( 'NONE', #6275, #4978, #267 ) ;
#6398 = DIRECTION ( 'NONE',  ( -0.000000000000000000, -0.000000000000000000, 1.000000000000000000 ) ) ;
#6399 = DIRECTION ( 'NONE',  ( 0.000000000000000000, 1.000000000000000000, 0.000000000000000000 ) ) ;
#6400 = ORIENTED_EDGE ( 'NONE', *, *, #1762, .T. ) ;
#6401 = ORIENTED_EDGE ( 'NONE', *, *, #3375, .T. ) ;
#6402 = CARTESIAN_POINT ( 'NONE',  ( 2.756197834950227410, 3.027510591568626896, -3.223146290109805356 ) ) ;
#6403 = EDGE_CURVE ( 'NONE', #1514, #7097, #6561, .T. ) ;
#6404 = DIRECTION ( 'NONE',  ( 0.000000000000000000, 1.000000000000000000, 0.000000000000000000 ) ) ;
#6405 = CARTESIAN_POINT ( 'NONE',  ( 20.00000000000000000, 140.0000000000000000, 40.00000000000000000 ) ) ;
#6406 = LINE ( 'NONE', #5796, #4996 ) ;
#6407 = CARTESIAN_POINT ( 'NONE',  ( 0.000000000000000000, 0.000000000000000000, 120.0000000000000000 ) ) ;
#6408 = EDGE_CURVE ( 'NONE', #3015, #6071, #5631, .T. ) ;
#6409 = VERTEX_POINT ( 'NONE', #2342 ) ;
#6410 = STYLED_ITEM ( 'NONE', ( #2659 ), #6254 ) ;
#6411 = CARTESIAN_POINT ( 'NONE',  ( 439.9999999999999432, -20.00000000000000000, 18.96857495968446017 ) ) ;
#6412 = CARTESIAN_POINT ( 'NONE',  ( 269.0000000000000000, 5.000000000000000000, 140.0000000000000000 ) ) ;
#6413 = CARTESIAN_POINT ( 'NONE',  ( 439.9999999999999432, -20.00000000000000000, 16.31857495968447225 ) ) ;
#6414 = LINE ( 'NONE', #455, #322 ) ;
#6415 = APPLICATION_CONTEXT ( 'automotive_design' ) ;
#6416 = AXIS2_PLACEMENT_3D ( 'NONE', #1915, #2649, #1334 ) ;
#6417 = MECHANICAL_DESIGN_GEOMETRIC_PRESENTATION_REPRESENTATION (  '', ( #5302 ), #5993 ) ;
#6418 = VERTEX_POINT ( 'NONE', #6327 ) ;
#6419 = CARTESIAN_POINT ( 'NONE',  ( 10.00000000000000000, 0.000000000000000000, -115.0000000000000000 ) ) ;
#6420 = ORIENTED_EDGE ( 'NONE', *, *, #400, .F. ) ;
#6421 =( LENGTH_UNIT ( ) NAMED_UNIT ( * ) SI_UNIT ( .MILLI., .METRE. ) );
#6422 = CARTESIAN_POINT ( 'NONE',  ( -4.000000000000000000, 0.9868501483902560878, -0.09357334158579519445 ) ) ;
#6423 = ITEM_DEFINED_TRANSFORMATION ( 'NONE', 'NONE', #7534,  #594 ) ;
#6424 = ORIENTED_EDGE ( 'NONE', *, *, #5376, .T. ) ;
#6425 = EDGE_LOOP ( 'NONE', ( #7302, #7337, #6948, #341 ) ) ;
#6426 = PLANE ( 'NONE',  #632 ) ;
#6427 = VECTOR ( 'NONE', #2928, 1000.000000000000000 ) ;
#6428 = DIRECTION ( 'NONE',  ( -0.000000000000000000, -0.000000000000000000, 1.000000000000000000 ) ) ;
#6429 = EDGE_CURVE ( 'NONE', #5755, #8497, #1067, .T. ) ;
#6430 = EDGE_CURVE ( 'NONE', #1428, #5070, #7556, .T. ) ;
#6431 = AXIS2_PLACEMENT_3D ( 'NONE', #5271, #5835, #1978 ) ;
#6432 = CARTESIAN_POINT ( 'NONE',  ( 170.9999999999999716, -4.999999999999998224, 145.0000000000000284 ) ) ;
#6433 = ORIENTED_EDGE ( 'NONE', *, *, #67, .F. ) ;
#6434 = AXIS2_PLACEMENT_3D ( 'NONE', #1662, #343, #5654 ) ;
#6435 = DIRECTION ( 'NONE',  ( 0.000000000000000000, 1.000000000000000000, 0.000000000000000000 ) ) ;
#6436 = DIRECTION ( 'NONE',  ( -1.000000000000000000, 0.000000000000000000, -0.000000000000000000 ) ) ;
#6437 = EDGE_LOOP ( 'NONE', ( #2623, #139, #544, #2687 ) ) ;
#6438 = AXIS2_PLACEMENT_3D ( 'NONE', #7081, #2484, #6469 ) ;
#6439 = EDGE_LOOP ( 'NONE', ( #4484, #6065 ) ) ;
#6440 = MECHANICAL_DESIGN_GEOMETRIC_PRESENTATION_REPRESENTATION (  '', ( #5315 ), #7551 ) ;
#6441 = DIRECTION ( 'NONE',  ( 0.000000000000000000, 0.000000000000000000, 1.000000000000000000 ) ) ;
#6442 = DIRECTION ( 'NONE',  ( -0.000000000000000000, -0.000000000000000000, 1.000000000000000000 ) ) ;
#6443 = EDGE_CURVE ( 'NONE', #5355, #2563, #1588, .T. ) ;
#6444 = VECTOR ( 'NONE', #7108, 1000.000000000000000 ) ;
#6445 = CARTESIAN_POINT ( 'NONE',  ( 269.0000000000000000, -4.999999999999998224, 139.9990000000000236 ) ) ;
#6446 = DIRECTION ( 'NONE',  ( -1.000000000000000000, 0.000000000000000000, 0.000000000000000000 ) ) ;
#6447 = EDGE_LOOP ( 'NONE', ( #6176, #838 ) ) ;
#6448 = VERTEX_POINT ( 'NONE', #7774 ) ;
#6449 = CARTESIAN_POINT ( 'NONE',  ( -0.1756481739660520902, 4.720212674038980261, -3.469390959564065291 ) ) ;
#6450 = VECTOR ( 'NONE', #3280, 1000.000000000000000 ) ;
#6451 = DIRECTION ( 'NONE',  ( -1.000000000000000000, 0.000000000000000000, -0.000000000000000000 ) ) ;
#6452 = DIRECTION ( 'NONE',  ( 0.000000000000000000, -1.000000000000000000, 0.000000000000000000 ) ) ;
#6453 = DIRECTION ( 'NONE',  ( -0.000000000000000000, 1.000000000000000000, -0.000000000000000000 ) ) ;
#6454 = DIRECTION ( 'NONE',  ( 0.000000000000000000, 0.000000000000000000, 1.000000000000000000 ) ) ;
#6455 = AXIS2_PLACEMENT_3D ( 'NONE', #8102, #5427, #3480 ) ;
#6456 = ORIENTED_EDGE ( 'NONE', *, *, #3426, .T. ) ;
#6457 = FACE_OUTER_BOUND ( 'NONE', #6149, .T. ) ;
#6458 = CARTESIAN_POINT ( 'NONE',  ( 303.3333333333333144, -14.99999999999999822, 162.5000000000000853 ) ) ;
#6459 = EDGE_CURVE ( 'NONE', #5070, #5424, #2473, .T. ) ;
#6460 = CARTESIAN_POINT ( 'NONE',  ( 4.000000000000000000, 2.309401076758515803, -0.4999999999999995559 ) ) ;
#6461 = ADVANCED_FACE ( 'NONE', ( #6623 ), #537, .T. ) ;
#6462 = EDGE_CURVE ( 'NONE', #7349, #590, #3953, .T. ) ;
#6463 = CARTESIAN_POINT ( 'NONE',  ( -30.00000000000000000, 15.00000000000000000, 145.0000000000000284 ) ) ;
#6464 = EDGE_LOOP ( 'NONE', ( #5659, #1918, #7963, #5512 ) ) ;
#6465 = DIRECTION ( 'NONE',  ( -0.000000000000000000, 1.000000000000000000, -0.000000000000000000 ) ) ;
#6466 = ITEM_DEFINED_TRANSFORMATION ( 'NONE', 'NONE', #5717,  #594 ) ;
#6467 = ORIENTED_EDGE ( 'NONE', *, *, #8369, .T. ) ;
#6468 = FACE_OUTER_BOUND ( 'NONE', #7586, .T. ) ;
#6469 = DIRECTION ( 'NONE',  ( 0.000000000000000000, 0.000000000000000000, 1.000000000000000000 ) ) ;
#6470 = VECTOR ( 'NONE', #5773, 1000.000000000000000 ) ;
#6471 = LINE ( 'NONE', #6340, #6470 ) ;
#6472 = ORIENTED_EDGE ( 'NONE', *, *, #4473, .T. ) ;
#6473 = DIRECTION ( 'NONE',  ( 1.000000000000000000, 0.000000000000000000, 0.000000000000000000 ) ) ;
#6474 = EDGE_CURVE ( 'NONE', #4765, #5053, #7231, .T. ) ;
#6475 = DIRECTION ( 'NONE',  ( 1.000000000000000000, 0.000000000000000000, 0.000000000000000000 ) ) ;
#6476 = CARTESIAN_POINT ( 'NONE',  ( 181.0000000000000000, -4.999999999999998224, 140.0000000000000000 ) ) ;
#6477 = VERTEX_POINT ( 'NONE', #3326 ) ;
#6478 = VERTEX_POINT ( 'NONE', #7856 ) ;
#6479 = CIRCLE ( 'NONE', #6193, 2.649999999999985700 ) ;
#6481 = VECTOR ( 'NONE', #6110, 1000.000000000000000 ) ;
#6480 = DIRECTION ( 'NONE',  ( -0.000000000000000000, 1.000000000000000000, -0.000000000000000000 ) ) ;
#6482 = EDGE_CURVE ( 'NONE', #7646, #3882, #7894, .T. ) ;
#6483 = CARTESIAN_POINT ( 'NONE',  ( 470.0000000000000000, -24.99999999999980105, 0.000000000000000000 ) ) ;
#6484 =( GEOMETRIC_REPRESENTATION_CONTEXT ( 3 ) GLOBAL_UNCERTAINTY_ASSIGNED_CONTEXT ( ( #8271 ) ) GLOBAL_UNIT_ASSIGNED_CONTEXT ( ( #2028, #4803, #5367 ) ) REPRESENTATION_CONTEXT ( 'NONE', 'WORKASPACE' ) );
#6485 = LINE ( 'NONE', #5136, #4111 ) ;
#6486 = AXIS2_PLACEMENT_3D ( 'NONE', #7742, #8516, #3207 ) ;
#6487 = FACE_OUTER_BOUND ( 'NONE', #6316, .T. ) ;
#6488 = EDGE_LOOP ( 'NONE', ( #5017, #4638 ) ) ;
#6489 = ORIENTED_EDGE ( 'NONE', *, *, #5641, .F. ) ;
#6490 = ORIENTED_EDGE ( 'NONE', *, *, #1538, .T. ) ;
#6491 = DIRECTION ( 'NONE',  ( 0.000000000000000000, -1.287488025362403787E-15, -1.000000000000000000 ) ) ;
#6492 = PRODUCT_RELATED_PRODUCT_CATEGORY ( 'part', '', ( #7953 ) ) ;
#6493 = PLANE ( 'NONE',  #2333 ) ;
#6494 = DIRECTION ( 'NONE',  ( -1.000000000000000000, -0.000000000000000000, -0.000000000000000000 ) ) ;
#6495 = CARTESIAN_POINT ( 'NONE',  ( 176.0000000000000000, -25.00000000000000000, -86.63142504031547730 ) ) ;
#6496 = CARTESIAN_POINT ( 'NONE',  ( -5.000000000000000000, -5.000000000000000000, 148.0000000000000284 ) ) ;
#6497 = SURFACE_STYLE_FILL_AREA ( #5107 ) ;
#6498 = DIRECTION ( 'NONE',  ( -0.000000000000000000, -0.000000000000000000, 1.000000000000000000 ) ) ;
#6499 = LINE ( 'NONE', #4501, #5861 ) ;
#6500 = EDGE_CURVE ( 'NONE', #342, #6268, #5151, .T. ) ;
#6501 = CARTESIAN_POINT ( 'NONE',  ( 5.000000000000000000, -5.000000000000000000, 148.0000000000000284 ) ) ;
#6502 = DIRECTION ( 'NONE',  ( 0.000000000000000000, 0.000000000000000000, 1.000000000000000000 ) ) ;
#6503 = EDGE_CURVE ( 'NONE', #3186, #8497, #6303, .T. ) ;
#6504 = ORIENTED_EDGE ( 'NONE', *, *, #4741, .T. ) ;
#6505 = FACE_OUTER_BOUND ( 'NONE', #8433, .T. ) ;
#6506 = EDGE_CURVE ( 'NONE', #2201, #2255, #576, .T. ) ;
#6507 = ORIENTED_EDGE ( 'NONE', *, *, #6764, .F. ) ;
#6508 = CARTESIAN_POINT ( 'NONE',  ( -30.00000000000002842, 786.6649314574284517, -200.0000000000000000 ) ) ;
#6509 = EDGE_CURVE ( 'NONE', #2303, #3508, #1813, .T. ) ;
#6510 = CARTESIAN_POINT ( 'NONE',  ( 5.000000000000001776, -4.999999999999998224, 139.9990000000000236 ) ) ;
#6511 = VECTOR ( 'NONE', #5264, 1000.000000000000000 ) ;
#6512 = PLANE ( 'NONE',  #7030 ) ;
#6513 = ORIENTED_EDGE ( 'NONE', *, *, #5601, .T. ) ;
#6514 = DIRECTION ( 'NONE',  ( 1.000000000000000000, 0.000000000000000000, 0.000000000000000000 ) ) ;
#6515 = CIRCLE ( 'NONE', #4991, 20.00000000000000000 ) ;
#6516 = SHAPE_DEFINITION_REPRESENTATION ( #1416, #2984 ) ;
#6517 = CARTESIAN_POINT ( 'NONE',  ( 0.000000000000000000, 0.000000000000000000, 120.0000000000000142 ) ) ;
#6518 = VERTEX_POINT ( 'NONE', #3937 ) ;
#6519 = ORIENTED_EDGE ( 'NONE', *, *, #1043, .T. ) ;
#6520 = LINE ( 'NONE', #559, #3380 ) ;
#6521 = DIRECTION ( 'NONE',  ( 0.000000000000000000, -0.000000000000000000, 1.000000000000000000 ) ) ;
#6522 = AXIS2_PLACEMENT_3D ( 'NONE', #8382, #6453, #5060 ) ;
#6523 = FACE_OUTER_BOUND ( 'NONE', #6367, .T. ) ;
#6524 = DIRECTION ( 'NONE',  ( -1.000000000000000000, 0.000000000000000000, 0.000000000000000000 ) ) ;
#6525 = EDGE_LOOP ( 'NONE', ( #7911, #78, #1066, #4866 ) ) ;
#6526 = ORIENTED_EDGE ( 'NONE', *, *, #4611, .F. ) ;
#6527 = AXIS2_PLACEMENT_3D ( 'NONE', #1319, #709, #2761 ) ;
#6528 = CARTESIAN_POINT ( 'NONE',  ( 386.6666666666666288, -25.00000000000000000, 165.1500000000000625 ) ) ;
#6529 = EDGE_CURVE ( 'NONE', #242, #6638, #3893, .T. ) ;
#6530 = ADVANCED_FACE ( 'NONE', ( #498, #1856 ), #7107, .T. ) ;
#6531 = PLANE ( 'NONE',  #3852 ) ;
#6532 = CARTESIAN_POINT ( 'NONE',  ( 347.0000000000000000, -4.999999999999998224, 140.0000000000000000 ) ) ;
#6533 = CARTESIAN_POINT ( 'NONE',  ( 0.000000000000000000, 0.000000000000000000, -84.56854249492380404 ) ) ;
#6534 = DIRECTION ( 'NONE',  ( -1.000000000000000000, 1.734723475976806848E-16, -0.000000000000000000 ) ) ;
#6535 = CARTESIAN_POINT ( 'NONE',  ( -5.000000000000000000, -5.000000000000000000, 140.0000000000000000 ) ) ;
#6536 = CARTESIAN_POINT ( 'NONE',  ( 4.000000000000000888, 1.563622288139206118, -0.2253451193528334950 ) ) ;
#6537 = ADVANCED_FACE ( 'NONE', ( #1154 ), #8474, .F. ) ;
#6538 = DIRECTION ( 'NONE',  ( 0.000000000000000000, 1.000000000000000000, 0.000000000000000000 ) ) ;
#6539 = DIRECTION ( 'NONE',  ( -1.000000000000000000, -0.000000000000000000, -0.000000000000000000 ) ) ;
#6540 = COLOUR_RGB ( '',0.8941176470588234615, 0.8941176470588234615, 0.8941176470588234615 ) ;
#6541 = ORIENTED_EDGE ( 'NONE', *, *, #6506, .F. ) ;
#6542 = CARTESIAN_POINT ( 'NONE',  ( -1.655952806101422814, 3.662737355149034979, -7.623296525288699970E-18 ) ) ;
#6543 = ORIENTED_EDGE ( 'NONE', *, *, #3748, .T. ) ;
#6544 = CARTESIAN_POINT ( 'NONE',  ( 2.000000000000000444, 3.464101615137754830, -3.142992957459231018 ) ) ;
#6545 = LINE ( 'NONE', #593, #1024 ) ;
#6546 = DIRECTION ( 'NONE',  ( 0.000000000000000000, -0.000000000000000000, 1.000000000000000000 ) ) ;
#6547 = PRODUCT_DEFINITION_CONTEXT ( 'detailed design', #7470, 'design' ) ;
#6548 = PLANE ( 'NONE',  #3845 ) ;
#6549 = ORIENTED_EDGE ( 'NONE', *, *, #3300, .F. ) ;
#6550 = DIRECTION ( 'NONE',  ( 0.000000000000000000, 0.000000000000000000, -1.000000000000000000 ) ) ;
#6551 =( LENGTH_UNIT ( ) NAMED_UNIT ( * ) SI_UNIT ( .MILLI., .METRE. ) );
#6552 = CARTESIAN_POINT ( 'NONE',  ( -1.654252653721913102, -3.663718938583024443, -0.01223254789874440342 ) ) ;
#6553 = ORIENTED_EDGE ( 'NONE', *, *, #6210, .T. ) ;
#6554 = MECHANICAL_DESIGN_GEOMETRIC_PRESENTATION_REPRESENTATION (  '', ( #581 ), #4753 ) ;
#6555 = ORIENTED_EDGE ( 'NONE', *, *, #5183, .T. ) ;
#6556 = FACE_OUTER_BOUND ( 'NONE', #5972, .T. ) ;
#6557 = DIRECTION ( 'NONE',  ( 0.000000000000000000, 1.000000000000000000, 0.000000000000000000 ) ) ;
#6558 = VECTOR ( 'NONE', #178, 1000.000000000000000 ) ;
#6559 = EDGE_CURVE ( 'NONE', #3262, #628, #7417, .T. ) ;
#6560 = AXIS2_PLACEMENT_3D ( 'NONE', #842, #5444, #2150 ) ;
#6561 = B_SPLINE_CURVE_WITH_KNOTS ( 'NONE', 3,
 ( #5064, #2986, #3682, #7025, #409, #8430 ),
 .UNSPECIFIED., .F., .F.,
 ( 4, 2, 4 ),
 ( 0.000000000000000000, 0.0002095117440854740156, 0.0004190234881709480313 ),
 .UNSPECIFIED. ) ;
#6562 = CARTESIAN_POINT ( 'NONE',  ( 4.000000000000000888, -0.8578082829538523635, -3.433262215449808696 ) ) ;
#6563 = CARTESIAN_POINT ( 'NONE',  ( -20.00000000000000000, 135.0000000000000000, 0.000000000000000000 ) ) ;
#6564 = VERTEX_POINT ( 'NONE', #8597 ) ;
#6565 = EDGE_CURVE ( 'NONE', #8255, #6478, #3242, .T. ) ;
#6566 =( GEOMETRIC_REPRESENTATION_CONTEXT ( 3 ) GLOBAL_UNCERTAINTY_ASSIGNED_CONTEXT ( ( #7997 ) ) GLOBAL_UNIT_ASSIGNED_CONTEXT ( ( #4947, #2942, #6986 ) ) REPRESENTATION_CONTEXT ( 'NONE', 'WORKASPACE' ) );
#6567 = SHAPE_REPRESENTATION_RELATIONSHIP ( 'NONE' , 'NONE' ,  #638, #1900 ) ;
#6568 = VERTEX_POINT ( 'NONE', #5232 ) ;
#6569 = LINE ( 'NONE', #3972, #2270 ) ;
#6570 = VECTOR ( 'NONE', #2581, 1000.000000000000114 ) ;
#6571 = VECTOR ( 'NONE', #5329, 1000.000000000000000 ) ;
#6572 = CARTESIAN_POINT ( 'NONE',  ( 53.33333333333330017, -20.00000000000000000, 162.5000000000000853 ) ) ;
#6573 = CARTESIAN_POINT ( 'NONE',  ( -5.560781378645575757, 6.809993116116508640E-16, -4.000000000000000000 ) ) ;
#6574 = VERTEX_POINT ( 'NONE', #4577 ) ;
#6575 = DIRECTION ( 'NONE',  ( 1.000000000000000000, 0.000000000000000000, 0.000000000000000000 ) ) ;
#6576 = APPLICATION_CONTEXT ( 'automotive_design' ) ;
#6577 = PRESENTATION_STYLE_ASSIGNMENT (( #4531 ) ) ;
#6578 = VECTOR ( 'NONE', #7987, 1000.000000000000000 ) ;
#6579 = ADVANCED_FACE ( 'NONE', ( #2627, #5270 ), #7940, .T. ) ;
#6580 = CARTESIAN_POINT ( 'NONE',  ( 0.000000000000000000, 0.000000000000000000, 140.0000000000000000 ) ) ;
#6581 = DIRECTION ( 'NONE',  ( 0.000000000000000000, 0.000000000000000000, 1.000000000000000000 ) ) ;
#6582 = CARTESIAN_POINT ( 'NONE',  ( 4.000000000000000000, 0.1981133338132474442, 2.382280164152719704E-17 ) ) ;
#6583 = VECTOR ( 'NONE', #3221, 1000.000000000000000 ) ;
#6584 = DIRECTION ( 'NONE',  ( 1.000000000000000000, 0.000000000000000000, -0.000000000000000000 ) ) ;
#6585 = DIRECTION ( 'NONE',  ( 1.000000000000000000, -1.734723475976806848E-16, 0.000000000000000000 ) ) ;
#6586 = CARTESIAN_POINT ( 'NONE',  ( -20.00000000000000000, 140.0000000000000000, 40.00000000000000000 ) ) ;
#6587 = ORIENTED_EDGE ( 'NONE', *, *, #8248, .F. ) ;
#6588 = ORIENTED_EDGE ( 'NONE', *, *, #1515, .F. ) ;
#6589 = ORIENTED_EDGE ( 'NONE', *, *, #8432, .F. ) ;
#6590 = CARTESIAN_POINT ( 'NONE',  ( 439.9999999999999432, -25.00000000000000000, 21.61857495968444454 ) ) ;
#6591 = PRODUCT_DEFINITION ( 'UNKNOWN', '', #4190, #5243 ) ;
#6592 = VECTOR ( 'NONE', #7202, 1000.000000000000000 ) ;
#6593 = DIRECTION ( 'NONE',  ( 1.734723475976807587E-16, 1.000000000000000000, 0.000000000000000000 ) ) ;
#6594 = DIRECTION ( 'NONE',  ( 0.000000000000000000, 1.000000000000000000, 0.000000000000000000 ) ) ;
#6595 = ORIENTED_EDGE ( 'NONE', *, *, #234, .F. ) ;
#6596 = DIRECTION ( 'NONE',  ( 0.000000000000000000, 0.000000000000000000, 1.000000000000000000 ) ) ;
#6597 = PRODUCT_CONTEXT ( 'NONE', #351, 'mechanical' ) ;
#6598 = CARTESIAN_POINT ( 'NONE',  ( 0.000000000000000000, 0.000000000000000000, 7.000000000000006217 ) ) ;
#6599 = VERTEX_POINT ( 'NONE', #834 ) ;
#6600 = EDGE_LOOP ( 'NONE', ( #7697, #4841, #8354, #2384 ) ) ;
#6601 = PLANE ( 'NONE',  #7830 ) ;
#6602 = DIRECTION ( 'NONE',  ( 0.000000000000000000, 0.000000000000000000, 1.000000000000000000 ) ) ;
#6603 = CARTESIAN_POINT ( 'NONE',  ( 352.0000000000000000, -20.00000000000000000, -13.58142504031548192 ) ) ;
#6604 = CYLINDRICAL_SURFACE ( 'NONE', #7204, 2.500000000000000444 ) ;
#6605 = ORIENTED_EDGE ( 'NONE', *, *, #1515, .T. ) ;
#6606 = AXIS2_PLACEMENT_3D ( 'NONE', #8524, #3297, #15 ) ;
#6607 = ADVANCED_FACE ( 'NONE', ( #1359 ), #5316, .F. ) ;
#6608 = ORIENTED_EDGE ( 'NONE', *, *, #6043, .F. ) ;
#6609 = CARTESIAN_POINT ( 'NONE',  ( 0.000000000000000000, 0.000000000000000000, -77.99999999999997158 ) ) ;
#6610 = EDGE_CURVE ( 'NONE', #2415, #6599, #7626, .T. ) ;
#6611 = EDGE_CURVE ( 'NONE', #8282, #3127, #2185, .T. ) ;
#6612 = CIRCLE ( 'NONE', #929, 2.649999999999985700 ) ;
#6613 = CIRCLE ( 'NONE', #6052, 2.499999999999999556 ) ;
#6614 = PLANE ( 'NONE',  #2050 ) ;
#6615 = CYLINDRICAL_SURFACE ( 'NONE', #3049, 2.649999999999985700 ) ;
#6616 = ORIENTED_EDGE ( 'NONE', *, *, #3379, .F. ) ;
#6617 = DIRECTION ( 'NONE',  ( -0.000000000000000000, -0.000000000000000000, 1.000000000000000000 ) ) ;
#6618 = LINE ( 'NONE', #3850, #1773 ) ;
#6619 = VECTOR ( 'NONE', #2427, 1000.000000000000000 ) ;
#6620 = VECTOR ( 'NONE', #8560, 1000.000000000000000 ) ;
#6621 = PRODUCT ( 'socket head cap screw_iso_ISO 4762 M5 x 20 - 20N', 'socket head cap screw_iso_ISO 4762 M5 x 20 - 20N', '', ( #906 ) ) ;
#6622 = DIRECTION ( 'NONE',  ( 0.000000000000000000, 1.000000000000000000, 0.000000000000000000 ) ) ;
#6623 = FACE_OUTER_BOUND ( 'NONE', #1216, .T. ) ;
#6624 = DIRECTION ( 'NONE',  ( -0.000000000000000000, -1.000000000000000000, -0.000000000000000000 ) ) ;
#6625 = FACE_OUTER_BOUND ( 'NONE', #6172, .T. ) ;
#6626 = FACE_OUTER_BOUND ( 'NONE', #3992, .T. ) ;
#6627 = DIRECTION ( 'NONE',  ( 1.000000000000000000, 0.000000000000000000, 0.000000000000000000 ) ) ;
#6628 = VERTEX_POINT ( 'NONE', #4225 ) ;
#6629 =( LENGTH_UNIT ( ) NAMED_UNIT ( * ) SI_UNIT ( .MILLI., .METRE. ) );
#6630 = EDGE_LOOP ( 'NONE', ( #786, #640, #991, #6589 ) ) ;
#6631 = ITEM_DEFINED_TRANSFORMATION ( 'NONE', 'NONE', #8240,  #594 ) ;
#6632 = ORIENTED_EDGE ( 'NONE', *, *, #1839, .F. ) ;
#6633 = CARTESIAN_POINT ( 'NONE',  ( -20.00000000000000000, 2.449293598294706513E-15, 120.0000000000000142 ) ) ;
#6634 = DIRECTION ( 'NONE',  ( 0.000000000000000000, -0.000000000000000000, 1.000000000000000000 ) ) ;
#6635 = EDGE_CURVE ( 'NONE', #3690, #989, #3574, .T. ) ;
#6636 = EDGE_CURVE ( 'NONE', #4134, #5482, #6876, .T. ) ;
#6637 = CARTESIAN_POINT ( 'NONE',  ( 264.0000000000000000, -25.00000000000000000, -51.43142504031546025 ) ) ;
#6638 = VERTEX_POINT ( 'NONE', #4021 ) ;
#6639 = PLANE ( 'NONE',  #2551 ) ;
#6640 = EDGE_CURVE ( 'NONE', #4446, #3415, #1614, .T. ) ;
#6641 = DIRECTION ( 'NONE',  ( -0.000000000000000000, -0.000000000000000000, 1.000000000000000000 ) ) ;
#6642 = CYLINDRICAL_SURFACE ( 'NONE', #5033, 20.00000000000000000 ) ;
#6643 = ORIENTED_EDGE ( 'NONE', *, *, #5606, .F. ) ;
#6644 = ORIENTED_EDGE ( 'NONE', *, *, #3010, .F. ) ;
#6645 = LINE ( 'NONE', #691, #6714 ) ;
#6646 = CIRCLE ( 'NONE', #3880, 10.00000000000000000 ) ;
#6647 = LINE ( 'NONE', #6687, #6583 ) ;
#6648 = CARTESIAN_POINT ( 'NONE',  ( 5.000000000000000000, -5.000000000000000000, -105.9999999999999858 ) ) ;
#6649 = VECTOR ( 'NONE', #2400, 1000.000000000000000 ) ;
#6650 = DIRECTION ( 'NONE',  ( 0.000000000000000000, 1.000000000000000000, 0.000000000000000000 ) ) ;
#6651 = EDGE_CURVE ( 'NONE', #4446, #5850, #5485, .T. ) ;
#6652 = EDGE_LOOP ( 'NONE', ( #941, #4524 ) ) ;
#6653 = ORIENTED_EDGE ( 'NONE', *, *, #934, .T. ) ;
#6654 = CARTESIAN_POINT ( 'NONE',  ( 0.000000000000000000, -20.00000000000000000, -157.5000000000000284 ) ) ;
#6655 = CIRCLE ( 'NONE', #119, 10.00000000000000000 ) ;
#6656 = CARTESIAN_POINT ( 'NONE',  ( 0.000000000000000000, 0.000000000000000000, 140.0000000000000000 ) ) ;
#6657 = LINE ( 'NONE', #1398, #1924 ) ;
#6658 = ORIENTED_EDGE ( 'NONE', *, *, #6886, .T. ) ;
#6659 = DIRECTION ( 'NONE',  ( 1.000000000000000000, 0.000000000000000000, 0.000000000000000000 ) ) ;
#6660 = ADVANCED_FACE ( 'NONE', ( #2836, #8285, #2276, #4268, #921, #8196, #8153, #4965, #4837, #2021, #878, #2323 ), #7489, .T. ) ;
#6661 = CARTESIAN_POINT ( 'NONE',  ( 0.000000000000000000, -1.178949249685213863, 2.042000000000002924 ) ) ;
#6662 = DIRECTION ( 'NONE',  ( 0.000000000000000000, 0.000000000000000000, -1.000000000000000000 ) ) ;
#6663 = AXIS2_PLACEMENT_3D ( 'NONE', #3784, #999, #5084 ) ;
#6664 = DIRECTION ( 'NONE',  ( 1.000000000000000000, 0.000000000000000000, 0.000000000000000000 ) ) ;
#6665 = CARTESIAN_POINT ( 'NONE',  ( -5.000000000000001776, 5.000000000000001776, -143.0000000000000284 ) ) ;
#6666 = CARTESIAN_POINT ( 'NONE',  ( 136.6666666666666288, -20.00000000000000000, 159.8500000000001080 ) ) ;
#6667 = ORIENTED_EDGE ( 'NONE', *, *, #6099, .T. ) ;
#6668 = SURFACE_SIDE_STYLE ('',( #1366 ) ) ;
#6669 = EDGE_CURVE ( 'NONE', #8497, #3186, #6727, .T. ) ;
#6670 = EDGE_LOOP ( 'NONE', ( #790, #6302, #6394, #645 ) ) ;
#6671 = UNCERTAINTY_MEASURE_WITH_UNIT (LENGTH_MEASURE( 1.000000000000000082E-05 ), #6629, 'distance_accuracy_value', 'NONE');
#6672 = ORIENTED_EDGE ( 'NONE', *, *, #2022, .F. ) ;
#6673 = FACE_OUTER_BOUND ( 'NONE', #3000, .T. ) ;
#6674 = CARTESIAN_POINT ( 'NONE',  ( 1.828356344711641102, 3.563200125723180900, -5.433716356636336675E-16 ) ) ;
#6675 = EDGE_LOOP ( 'NONE', ( #2494, #684 ) ) ;
#6676 = FACE_OUTER_BOUND ( 'NONE', #3503, .T. ) ;
#6677 = ORIENTED_EDGE ( 'NONE', *, *, #7146, .T. ) ;
#6678 = LINE ( 'NONE', #726, #1016 ) ;
#6679 = DIRECTION ( 'NONE',  ( 0.000000000000000000, 0.000000000000000000, 1.000000000000000000 ) ) ;
#6680 = DIRECTION ( 'NONE',  ( 5.204170427930421283E-18, -1.000000000000000000, 5.551115123125782702E-17 ) ) ;
#6681 = CARTESIAN_POINT ( 'NONE',  ( -5.000000000000001776, 5.000000000000001776, 148.0000000000000284 ) ) ;
#6682 = ORIENTED_EDGE ( 'NONE', *, *, #7044, .T. ) ;
#6683 = ORIENTED_EDGE ( 'NONE', *, *, #2895, .F. ) ;
#6684 = EDGE_CURVE ( 'NONE', #3427, #7651, #4179, .T. ) ;
#6685 =( GEOMETRIC_REPRESENTATION_CONTEXT ( 3 ) GLOBAL_UNCERTAINTY_ASSIGNED_CONTEXT ( ( #5759 ) ) GLOBAL_UNIT_ASSIGNED_CONTEXT ( ( #349, #8373, #5661 ) ) REPRESENTATION_CONTEXT ( 'NONE', 'WORKASPACE' ) );
#6686 = LINE ( 'NONE', #4517, #6151 ) ;
#6687 = CARTESIAN_POINT ( 'NONE',  ( 5.000000000000000000, -5.000000000000000000, -27.99999999999999645 ) ) ;
#6688 = CARTESIAN_POINT ( 'NONE',  ( 0.000000000000000000, 0.000000000000000000, -27.99999999999999645 ) ) ;
#6689 = AXIS2_PLACEMENT_3D ( 'NONE', #7832, #7299, #5289 ) ;
#6690 = PRODUCT ( 'roller axis assy_r2', 'roller axis assy_r2', '', ( #1214 ) ) ;
#6691 = CYLINDRICAL_SURFACE ( 'NONE', #4012, 2.649999999999985700 ) ;
#6692 = VERTEX_POINT ( 'NONE', #7533 ) ;
#6693 = COLOUR_RGB ( '',0.8941176470588234615, 0.8941176470588234615, 0.8941176470588234615 ) ;
#6694 = VERTEX_POINT ( 'NONE', #4922 ) ;
#6695 = AXIS2_PLACEMENT_3D ( 'NONE', #4185, #6662, #6844 ) ;
#6696 = PLANE ( 'NONE',  #458 ) ;
#6697 = PRODUCT_RELATED_PRODUCT_CATEGORY ( 'part', '', ( #6690 ) ) ;
#6698 = CIRCLE ( 'NONE', #871, 2.649999999999985700 ) ;
#6699 = DIRECTION ( 'NONE',  ( 0.000000000000000000, 0.000000000000000000, 1.000000000000000000 ) ) ;
#6700 = CARTESIAN_POINT ( 'NONE',  ( 386.6666666666666288, -15.00000000000000000, 162.5000000000000853 ) ) ;
#6701 = ORIENTED_EDGE ( 'NONE', *, *, #1949, .T. ) ;
#6702 = FACE_OUTER_BOUND ( 'NONE', #7171, .T. ) ;
#6703 = VECTOR ( 'NONE', #8056, 1000.000000000000000 ) ;
#6704 = CIRCLE ( 'NONE', #4769, 2.649999999999985700 ) ;
#6705 = CARTESIAN_POINT ( 'NONE',  ( 0.000000000000000000, 0.000000000000000000, -77.99999999999997158 ) ) ;
#6706 = CIRCLE ( 'NONE', #2966, 2.649999999999985700 ) ;
#6707 = PLANE ( 'NONE',  #724 ) ;
#6708 = PLANE ( 'NONE',  #2376 ) ;
#6709 = AXIS2_PLACEMENT_3D ( 'NONE', #3630, #6286, #3723 ) ;
#6710 = CYLINDRICAL_SURFACE ( 'NONE', #4711, 10.00000000000000000 ) ;
#6711 = FACE_BOUND ( 'NONE', #2652, .T. ) ;
#6712 = AXIS2_PLACEMENT_3D ( 'NONE', #1458, #4115, #2076 ) ;
#6713 = ORIENTED_EDGE ( 'NONE', *, *, #1847, .F. ) ;
#6714 = VECTOR ( 'NONE', #4692, 1000.000000000000000 ) ;
#6715 = EDGE_LOOP ( 'NONE', ( #4616, #5702, #3432, #6201 ) ) ;
#6716 = EDGE_CURVE ( 'NONE', #5045, #5286, #3531, .T. ) ;
#6717 = ORIENTED_EDGE ( 'NONE', *, *, #5771, .F. ) ;
#6718 = CARTESIAN_POINT ( 'NONE',  ( 219.9999999999999716, -25.00000000000000000, 165.1500000000000625 ) ) ;
#6719 = EDGE_CURVE ( 'NONE', #4392, #4319, #6918, .T. ) ;
#6720 = DIRECTION ( 'NONE',  ( 0.000000000000000000, 1.000000000000000000, 0.000000000000000000 ) ) ;
#6721 = VECTOR ( 'NONE', #162, 1000.000000000000000 ) ;
#6722 = EDGE_CURVE ( 'NONE', #6999, #1077, #6264, .T. ) ;
#6723 = ORIENTED_EDGE ( 'NONE', *, *, #5359, .T. ) ;
#6724 = DIRECTION ( 'NONE',  ( -1.000000000000000000, -0.000000000000000000, -0.000000000000000000 ) ) ;
#6725 = VERTEX_POINT ( 'NONE', #6960 ) ;
#6726 = DIRECTION ( 'NONE',  ( -1.000000000000000000, 0.000000000000000000, 0.000000000000000000 ) ) ;
#6727 = CIRCLE ( 'NONE', #2988, 2.649999999999985700 ) ;
#6728 = LINE ( 'NONE', #18, #6339 ) ;
#6729 = CONTEXT_DEPENDENT_SHAPE_REPRESENTATION ( #1529, #5990 ) ;
#6730 = CARTESIAN_POINT ( 'NONE',  ( -2.500000000000000444, 3.061616997868383634E-16, -5.000000000000000888 ) ) ;
#6731 = ORIENTED_EDGE ( 'NONE', *, *, #2060, .T. ) ;
#6732 = ORIENTED_EDGE ( 'NONE', *, *, #7280, .T. ) ;
#6733 = FACE_OUTER_BOUND ( 'NONE', #3841, .T. ) ;
#6734 = DIRECTION ( 'NONE',  ( -0.000000000000000000, 1.000000000000000000, -0.000000000000000000 ) ) ;
#6735 = DIRECTION ( 'NONE',  ( -0.000000000000000000, -0.000000000000000000, 1.000000000000000000 ) ) ;
#6736 = EDGE_CURVE ( 'NONE', #35, #428, #1003, .T. ) ;
#6737 = DIRECTION ( 'NONE',  ( 0.8660254037844374864, -0.5000000000000018874, 0.000000000000000000 ) ) ;
#6738 = ORIENTED_EDGE ( 'NONE', *, *, #7099, .T. ) ;
#6739 = FILL_AREA_STYLE ('',( #1523 ) ) ;
#6740 = CARTESIAN_POINT ( 'NONE',  ( 386.6666666666666288, -20.00000000000000000, 159.8500000000001080 ) ) ;
#6741 = ORIENTED_EDGE ( 'NONE', *, *, #5798, .T. ) ;
#6742 = ORIENTED_EDGE ( 'NONE', *, *, #2829, .F. ) ;
#6743 = CARTESIAN_POINT ( 'NONE',  ( 10.00000000000000000, 0.000000000000000000, 140.0000000000000000 ) ) ;
#6744 = APPLICATION_CONTEXT ( 'automotive_design' ) ;
#6745 = AXIS2_PLACEMENT_3D ( 'NONE', #2413, #3791, #7801 ) ;
#6746 = DIRECTION ( 'NONE',  ( 0.000000000000000000, 0.000000000000000000, -1.000000000000000000 ) ) ;
#6747 = DIRECTION ( 'NONE',  ( 1.000000000000000000, 0.000000000000000000, 0.000000000000000000 ) ) ;
#6748 = ORIENTED_EDGE ( 'NONE', *, *, #4033, .F. ) ;
#6749 = CARTESIAN_POINT ( 'NONE',  ( -5.000000000000000000, -5.000000000000000000, 148.0000000000000284 ) ) ;
#6750 = EDGE_CURVE ( 'NONE', #2735, #3700, #2672, .T. ) ;
#6751 = PLANE ( 'NONE',  #8247 ) ;
#6752 = VECTOR ( 'NONE', #5719, 1000.000000000000000 ) ;
#6753 = CIRCLE ( 'NONE', #1339, 2.649999999999985700 ) ;
#6754 = CARTESIAN_POINT ( 'NONE',  ( 20.00000000000000000, 0.000000000000000000, 120.0000000000000142 ) ) ;
#6755 = DIRECTION ( 'NONE',  ( 0.000000000000000000, 0.000000000000000000, 1.000000000000000000 ) ) ;
#6756 = AXIS2_PLACEMENT_3D ( 'NONE', #5885, #5838, #1982 ) ;
#6757 = CARTESIAN_POINT ( 'NONE',  ( -20.00000000000000000, 2.449293598294706513E-15, -120.5685424949237898 ) ) ;
#6758 = LINE ( 'NONE', #2849, #4126 ) ;
#6759 = AXIS2_PLACEMENT_3D ( 'NONE', #3847, #6404, #2506 ) ;
#6760 = ORIENTED_EDGE ( 'NONE', *, *, #6443, .F. ) ;
#6761 = VERTEX_POINT ( 'NONE', #6396 ) ;
#6762 = EDGE_LOOP ( 'NONE', ( #1331, #8310 ) ) ;
#6763 = DIRECTION ( 'NONE',  ( -1.734723475976806848E-16, 1.000000000000000000, 0.000000000000000000 ) ) ;
#6764 = EDGE_CURVE ( 'NONE', #5482, #3613, #5818, .T. ) ;
#6765 =( NAMED_UNIT ( * ) SI_UNIT ( $, .STERADIAN. ) SOLID_ANGLE_UNIT ( ) );
#6766 = PRODUCT_DEFINITION_SHAPE ( 'NONE', 'NONE',  #7879 ) ;
#6767 = ORIENTED_EDGE ( 'NONE', *, *, #1684, .F. ) ;
#6768 = DIRECTION ( 'NONE',  ( -1.734723475976806848E-16, 1.000000000000000000, 0.000000000000000000 ) ) ;
#6769 = ORIENTED_EDGE ( 'NONE', *, *, #4611, .T. ) ;
#6770 = DIRECTION ( 'NONE',  ( -0.000000000000000000, 1.000000000000000000, -0.000000000000000000 ) ) ;
#6771 = LINE ( 'NONE', #3473, #6481 ) ;
#6772 = CONTEXT_DEPENDENT_SHAPE_REPRESENTATION ( #7191, #4829 ) ;
#6773 =( NAMED_UNIT ( * ) PLANE_ANGLE_UNIT ( ) SI_UNIT ( $, .RADIAN. ) );
#6774 = ORIENTED_EDGE ( 'NONE', *, *, #5995, .F. ) ;
#6775 = EDGE_CURVE ( 'NONE', #5009, #1117, #1706, .T. ) ;
#6776 = ORIENTED_EDGE ( 'NONE', *, *, #580, .T. ) ;
#6777 = LINE ( 'NONE', #5386, #7544 ) ;
#6778 = LINE ( 'NONE', #7572, #5754 ) ;
#6779 = CYLINDRICAL_SURFACE ( 'NONE', #7165, 2.649999999999985700 ) ;
#6780 = LINE ( 'NONE', #2173, #1373 ) ;
#6781 = VERTEX_POINT ( 'NONE', #3094 ) ;
#6782 = LINE ( 'NONE', #7483, #1642 ) ;
#6783 = FILL_AREA_STYLE ('',( #3527 ) ) ;
#6784 = DIRECTION ( 'NONE',  ( -0.000000000000000000, 1.000000000000000000, -0.000000000000000000 ) ) ;
#6785 = ORIENTED_EDGE ( 'NONE', *, *, #7926, .T. ) ;
#6786 = ORIENTED_EDGE ( 'NONE', *, *, #5181, .T. ) ;
#6787 = CARTESIAN_POINT ( 'NONE',  ( 4.000000000000000000, 2.309401076758497151, -5.000000000000000000 ) ) ;
#6788 = VECTOR ( 'NONE', #7010, 1000.000000000000000 ) ;
#6789 = CARTESIAN_POINT ( 'NONE',  ( 136.6666666666666288, -20.00000000000000000, 162.5000000000000853 ) ) ;
#6790 = FACE_BOUND ( 'NONE', #3137, .T. ) ;
#6791 = ORIENTED_EDGE ( 'NONE', *, *, #2271, .T. ) ;
#6792 = DIRECTION ( 'NONE',  ( 0.000000000000000000, 0.8660254037844380415, -0.5000000000000011102 ) ) ;
#6793 = AXIS2_PLACEMENT_3D ( 'NONE', #8147, #4260, #7394 ) ;
#6794 = DIRECTION ( 'NONE',  ( -0.000000000000000000, 1.000000000000000000, -0.000000000000000000 ) ) ;
#6795 = EDGE_CURVE ( 'NONE', #1514, #3609, #432, .T. ) ;
#6796 = EDGE_CURVE ( 'NONE', #5505, #479, #7051, .T. ) ;
#6797 = DIRECTION ( 'NONE',  ( -0.7071067811865306973, 8.659560562355138702E-17, -0.7071067811865643371 ) ) ;
#6798 = CARTESIAN_POINT ( 'NONE',  ( 0.000000000000000000, 0.000000000000000000, -63.99999999999997158 ) ) ;
#6799 = CARTESIAN_POINT ( 'NONE',  ( -1.287237434361707233, -3.875615274277397937, -3.430618716626816500 ) ) ;
#6800 = CARTESIAN_POINT ( 'NONE',  ( 0.000000000000000000, 0.000000000000000000, -5.000000000000000888 ) ) ;
#6801 = ORIENTED_EDGE ( 'NONE', *, *, #8466, .F. ) ;
#6802 = ORIENTED_EDGE ( 'NONE', *, *, #2896, .T. ) ;
#6803 = VERTEX_POINT ( 'NONE', #1219 ) ;
#6804 = CARTESIAN_POINT ( 'NONE',  ( 176.0000000000000000, -25.00000000000000000, -83.98142504031548583 ) ) ;
#6805 = AXIS2_PLACEMENT_3D ( 'NONE', #4529, #4411, #1891 ) ;
#6806 = DIRECTION ( 'NONE',  ( -1.000000000000000000, -0.000000000000000000, -0.000000000000000000 ) ) ;
#6807 = ADVANCED_FACE ( 'NONE', ( #3140 ), #7006, .F. ) ;
#6808 =( BOUNDED_SURFACE ( )  B_SPLINE_SURFACE ( 3, 2, ( 
 ( #7725, #3104, #8376 ),
 ( #1187, #2541, #7847 ),
 ( #6402, #3843, #3188 ),
 ( #3669, #1756, #1101 ),
 ( #6360, #3711, #2502 ),
 ( #6449, #5664, #396 ) ),
 .UNSPECIFIED., .F., .F., .T. ) 
 B_SPLINE_SURFACE_WITH_KNOTS ( ( 4, 2, 4 ),
 ( 3, 3 ),
 ( 0.02032853247518126225, 0.02278863295364821212, 0.02524873343211516200 ),
 ( 0.000000000000000000, 1.000000000000000000 ),
 .UNSPECIFIED. ) 
 GEOMETRIC_REPRESENTATION_ITEM ( )  RATIONAL_B_SPLINE_SURFACE ( (
 ( 1.000000000000000000, 0.8047781615896835161, 1.000000000000000000),
 ( 1.000000000000000000, 0.8123767586291043008, 1.000000000000000000),
 ( 1.000000000000000000, 0.8190662415562011134, 1.000000000000000000),
 ( 1.000000000000000000, 0.8192361015671398849, 1.000000000000000000),
 ( 1.000000000000000000, 0.8126135807102121689, 1.000000000000000000),
 ( 1.000000000000000000, 0.8047712338318585568, 1.000000000000000000) ) ) 
 REPRESENTATION_ITEM ( '' )  SURFACE ( )  );
#6809 = VERTEX_POINT ( 'NONE', #6483 ) ;
#6810 = CARTESIAN_POINT ( 'NONE',  ( -5.000000000000000000, -5.000000000000000000, 148.0000000000000284 ) ) ;
#6811 = ORIENTED_EDGE ( 'NONE', *, *, #1626, .T. ) ;
#6812 = DIRECTION ( 'NONE',  ( 1.000000000000000000, 0.000000000000000000, 0.000000000000000000 ) ) ;
#6813 = DIRECTION ( 'NONE',  ( 0.000000000000000000, 0.000000000000000000, 1.000000000000000000 ) ) ;
#6814 = CONTEXT_DEPENDENT_SHAPE_REPRESENTATION ( #634, #6064 ) ;
#6815 = LINE ( 'NONE', #1384, #7111 ) ;
#6816 = ORIENTED_EDGE ( 'NONE', *, *, #1488, .F. ) ;
#6817 = EDGE_LOOP ( 'NONE', ( #8576, #4095 ) ) ;
#6818 = DIRECTION ( 'NONE',  ( -1.734723475976806848E-16, 1.000000000000000000, 0.000000000000000000 ) ) ;
#6819 = DIRECTION ( 'NONE',  ( -1.000000000000000000, 0.000000000000000000, 0.000000000000000000 ) ) ;
#6820 = B_SPLINE_CURVE_WITH_KNOTS ( 'NONE', 3,
 ( #3176, #4643, #2572, #5339, #7300, #6552, #688, #3302 ),
 .UNSPECIFIED., .F., .F.,
 ( 4, 2, 2, 4 ),
 ( 2.465131517390770070E-07, 0.001183067374689869946, 0.001774477805458935659, 0.002365888236228001588 ),
 .UNSPECIFIED. ) ;
#6821 = CARTESIAN_POINT ( 'NONE',  ( 269.0000000000000000, -4.999999999999998224, 139.9990000000000236 ) ) ;
#6822 = LINE ( 'NONE', #2828, #6931 ) ;
#6823 = ORIENTED_EDGE ( 'NONE', *, *, #5078, .T. ) ;
#6824 = PRESENTATION_LAYER_ASSIGNMENT (  '', '', ( #3632 ) ) ;
#6825 =( NAMED_UNIT ( * ) PLANE_ANGLE_UNIT ( ) SI_UNIT ( $, .RADIAN. ) );
#6826 = CARTESIAN_POINT ( 'NONE',  ( -4.211140560182196957, -2.431303136016552013, -3.745885042887436178 ) ) ;
#6827 = VERTEX_POINT ( 'NONE', #5089 ) ;
#6828 = ORIENTED_EDGE ( 'NONE', *, *, #8287, .T. ) ;
#6829 = EDGE_CURVE ( 'NONE', #6564, #1248, #7759, .T. ) ;
#6830 = CARTESIAN_POINT ( 'NONE',  ( 303.3333333333333144, -25.00000000000000000, 165.1500000000000625 ) ) ;
#6831 = CARTESIAN_POINT ( 'NONE',  ( -5.000000000000001776, 5.000000000000001776, 148.0000000000000284 ) ) ;
#6832 = EDGE_CURVE ( 'NONE', #6599, #5850, #7840, .T. ) ;
#6833 = AXIS2_PLACEMENT_3D ( 'NONE', #2403, #6344, #2490 ) ;
#6834 = COLOUR_RGB ( '',0.8941176470588234615, 0.8941176470588234615, 0.8941176470588234615 ) ;
#6835 = ADVANCED_FACE ( 'NONE', ( #4518 ), #3055, .T. ) ;
#6836 = CARTESIAN_POINT ( 'NONE',  ( 0.000000000000000000, 0.000000000000000000, -4.000000000000000000 ) ) ;
#6837 = CARTESIAN_POINT ( 'NONE',  ( 0.000000000000000000, 0.000000000000000000, 27.00000000000001066 ) ) ;
#6838 = ORIENTED_EDGE ( 'NONE', *, *, #1392, .T. ) ;
#6839 = FACE_OUTER_BOUND ( 'NONE', #5684, .T. ) ;
#6840 = SURFACE_STYLE_USAGE ( .BOTH. , #3667 ) ;
#6841 = PRODUCT_DEFINITION_SHAPE ( 'NONE', 'NONE',  #8613 ) ;
#6842 = CARTESIAN_POINT ( 'NONE',  ( 3.245314017740480046E-16, -20.00000000000000000, -160.1500000000000057 ) ) ;
#6843 = AXIS2_PLACEMENT_3D ( 'NONE', #3364, #2102, #4752 ) ;
#6844 = DIRECTION ( 'NONE',  ( -1.000000000000000000, 0.000000000000000000, 0.000000000000000000 ) ) ;
#6845 = VECTOR ( 'NONE', #744, 1000.000000000000000 ) ;
#6846 = DIRECTION ( 'NONE',  ( -1.734723475976806848E-16, 1.000000000000000000, 0.000000000000000000 ) ) ;
#6847 = VECTOR ( 'NONE', #4224, 1000.000000000000000 ) ;
#6848 = CARTESIAN_POINT ( 'NONE',  ( 4.000000000000000000, 2.309401076758515803, -0.4999999999999995559 ) ) ;
#6849 = PLANE ( 'NONE',  #2872 ) ;
#6850 = EDGE_CURVE ( 'NONE', #4209, #5979, #6310, .T. ) ;
#6851 = VERTEX_POINT ( 'NONE', #344 ) ;
#6852 = ORIENTED_EDGE ( 'NONE', *, *, #4872, .F. ) ;
#6853 = CARTESIAN_POINT ( 'NONE',  ( 2.171643655288379993, -3.365003104552334978, -1.195831703456429434E-14 ) ) ;
#6854 = DIRECTION ( 'NONE',  ( -1.000000000000000000, 0.000000000000000000, 0.000000000000000000 ) ) ;
#6855 = SURFACE_STYLE_USAGE ( .BOTH. , #6152 ) ;
#6856 = AXIS2_PLACEMENT_3D ( 'NONE', #509, #7660, #2398 ) ;
#6857 = VERTEX_POINT ( 'NONE', #3789 ) ;
#6858 = AXIS2_PLACEMENT_3D ( 'NONE', #2822, #3519, #6114 ) ;
#6859 = CARTESIAN_POINT ( 'NONE',  ( -30.00000000000002842, -20.00000000000000000, 200.0000000000000000 ) ) ;
#6860 = ORIENTED_EDGE ( 'NONE', *, *, #7281, .F. ) ;
#6861 = APPLICATION_CONTEXT ( 'automotive_design' ) ;
#6862 = DIRECTION ( 'NONE',  ( -1.000000000000000000, 0.000000000000000000, -0.000000000000000000 ) ) ;
#6863 = EDGE_LOOP ( 'NONE', ( #2985, #8347 ) ) ;
#6864 = ORIENTED_EDGE ( 'NONE', *, *, #7218, .F. ) ;
#6865 = AXIS2_PLACEMENT_3D ( 'NONE', #7421, #4196, #6763 ) ;
#6866 = DIRECTION ( 'NONE',  ( -1.000000000000000000, -0.000000000000000000, -0.000000000000000000 ) ) ;
#6867 = DIRECTION ( 'NONE',  ( 0.000000000000000000, 0.000000000000000000, 1.000000000000000000 ) ) ;
#6868 = AXIS2_PLACEMENT_3D ( 'NONE', #4664, #7326, #1528 ) ;
#6869 = CARTESIAN_POINT ( 'NONE',  ( 0.000000000000000000, 0.000000000000000000, 7.000000000000006217 ) ) ;
#6870 = FACE_OUTER_BOUND ( 'NONE', #6346, .T. ) ;
#6871 = ORIENTED_EDGE ( 'NONE', *, *, #3689, .T. ) ;
#6872 =( NAMED_UNIT ( * ) SI_UNIT ( $, .STERADIAN. ) SOLID_ANGLE_UNIT ( ) );
#6873 = CARTESIAN_POINT ( 'NONE',  ( 0.000000000000000000, 0.000000000000000000, -115.0000000000000000 ) ) ;
#6874 = ORIENTED_EDGE ( 'NONE', *, *, #6319, .F. ) ;
#6875 = CARTESIAN_POINT ( 'NONE',  ( -3.436319922987618902, 2.634841920961291439, -3.531542292955721862 ) ) ;
#6876 = LINE ( 'NONE', #4312, #6721 ) ;
#6877 = AXIS2_PLACEMENT_3D ( 'NONE', #7999, #2682, #5976 ) ;
#6878 = EDGE_CURVE ( 'NONE', #4350, #1995, #5656, .T. ) ;
#6879 = DIRECTION ( 'NONE',  ( 0.000000000000000000, 0.000000000000000000, 1.000000000000000000 ) ) ;
#6880 = EDGE_CURVE ( 'NONE', #1609, #4852, #1134, .T. ) ;
#6881 = DIRECTION ( 'NONE',  ( 1.000000000000000000, 0.000000000000000000, 0.000000000000000000 ) ) ;
#6882 = EDGE_LOOP ( 'NONE', ( #4550, #7418, #2766, #6472 ) ) ;
#6883 = CARTESIAN_POINT ( 'NONE',  ( 470.0000000000000000, 15.00000000000000000, 145.0000000000000284 ) ) ;
#6884 = EDGE_CURVE ( 'NONE', #1660, #678, #5782, .T. ) ;
#6885 = CARTESIAN_POINT ( 'NONE',  ( 0.000000000000000000, 0.000000000000000000, 0.000000000000000000 ) ) ;
#6886 = EDGE_CURVE ( 'NONE', #7751, #4379, #7423, .T. ) ;
#6887 = PLANE ( 'NONE',  #5448 ) ;
#6888 = AXIS2_PLACEMENT_3D ( 'NONE', #7181, #1220, #5866 ) ;
#6889 = DIRECTION ( 'NONE',  ( -1.000000000000000000, -0.000000000000000000, -0.000000000000000000 ) ) ;
#6890 = CARTESIAN_POINT ( 'NONE',  ( -4.000000000000000000, 2.309401076758498483, -3.433295621305379353 ) ) ;
#6891 = VERTEX_POINT ( 'NONE', #6350 ) ;
#6892 = CIRCLE ( 'NONE', #8021, 20.00000000000000000 ) ;
#6893 = ORIENTED_EDGE ( 'NONE', *, *, #2002, .T. ) ;
#6894 = ORIENTED_EDGE ( 'NONE', *, *, #2810, .F. ) ;
#6895 = CARTESIAN_POINT ( 'NONE',  ( 0.000000000000000000, 0.000000000000000000, 27.00000000000000711 ) ) ;
#6896 = DIRECTION ( 'NONE',  ( 1.000000000000000000, 0.000000000000000000, 0.000000000000000000 ) ) ;
#6897 = AXIS2_PLACEMENT_3D ( 'NONE', #6800, #5497, #8126 ) ;
#6898 = ORIENTED_EDGE ( 'NONE', *, *, #4396, .F. ) ;
#6899 = DIRECTION ( 'NONE',  ( 0.000000000000000000, 0.000000000000000000, 1.000000000000000000 ) ) ;
#6900 = VERTEX_POINT ( 'NONE', #1834 ) ;
#6901 = DIRECTION ( 'NONE',  ( -0.000000000000000000, 1.000000000000000000, -0.000000000000000000 ) ) ;
#6902 = ORIENTED_EDGE ( 'NONE', *, *, #2895, .T. ) ;
#6903 = ORIENTED_EDGE ( 'NONE', *, *, #14, .T. ) ;
#6904 =( GEOMETRIC_REPRESENTATION_CONTEXT ( 3 ) GLOBAL_UNCERTAINTY_ASSIGNED_CONTEXT ( ( #5918 ) ) GLOBAL_UNIT_ASSIGNED_CONTEXT ( ( #665, #2787, #5431 ) ) REPRESENTATION_CONTEXT ( 'NONE', 'WORKASPACE' ) );
#6906 = CIRCLE ( 'NONE', #2459, 2.500000000000000888 ) ;
#6905 = LINE ( 'NONE', #1430, #456 ) ;
#6907 = CARTESIAN_POINT ( 'NONE',  ( -3.333333333333335258, 2.694301256218251783, -3.300726591567079815 ) ) ;
#6908 = EDGE_CURVE ( 'NONE', #3700, #1248, #388, .T. ) ;
#6909 = EDGE_CURVE ( 'NONE', #1995, #3708, #4507, .T. ) ;
#6910 = ADVANCED_FACE ( 'NONE', ( #3180 ), #7137, .F. ) ;
#6911 = CARTESIAN_POINT ( 'NONE',  ( -2.449848172108560540, -3.432307619358754724, -3.503702292528910078 ) ) ;
#6912 = CARTESIAN_POINT ( 'NONE',  ( 0.6640947660595348800, -4.471078309994175548, -3.602146406945708090 ) ) ;
#6913 = ORIENTED_EDGE ( 'NONE', *, *, #201, .T. ) ;
#6914 = FACE_OUTER_BOUND ( 'NONE', #1290, .T. ) ;
#6915 = ORIENTED_EDGE ( 'NONE', *, *, #3194, .F. ) ;
#6916 = CARTESIAN_POINT ( 'NONE',  ( -2.807080416178626692, 3.225969019225154444, -3.502507215260441065 ) ) ;
#6917=STYLED_ITEM('',(#8643),#2263);
#6918 = LINE ( 'NONE', #965, #3539 ) ;
#6919 = EDGE_CURVE ( 'NONE', #7567, #2207, #5295, .T. ) ;
#6920 = CARTESIAN_POINT ( 'NONE',  ( -5.000000000000001776, 5.000000000000001776, 148.0000000000000284 ) ) ;
#6921 = CARTESIAN_POINT ( 'NONE',  ( 20.00000000000000000, 0.000000000000000000, 27.00000000000001066 ) ) ;
#6922 = EDGE_LOOP ( 'NONE', ( #947, #6588 ) ) ;
#6923 = DIRECTION ( 'NONE',  ( -0.000000000000000000, -0.000000000000000000, 1.000000000000000000 ) ) ;
#6924 = LINE ( 'NONE', #5491, #7964 ) ;
#6925 = AXIS2_PLACEMENT_3D ( 'NONE', #435, #5008, #5700 ) ;
#6926 = CARTESIAN_POINT ( 'NONE',  ( 10.00000000000000000, 0.000000000000000000, -77.99999999999997158 ) ) ;
#6927 = CARTESIAN_POINT ( 'NONE',  ( -20.00000000000000000, 2.449293598294706513E-15, -49.56854249492377562 ) ) ;
#6928 = ADVANCED_FACE ( 'NONE', ( #606 ), #2007, .F. ) ;
#6929 = DIRECTION ( 'NONE',  ( 1.000000000000000000, 0.000000000000000000, 0.000000000000000000 ) ) ;
#6930 = CARTESIAN_POINT ( 'NONE',  ( -4.197312064133472020, -0.8182229787990021874, -3.502518405183886685 ) ) ;
#6931 = VECTOR ( 'NONE', #2268, 1000.000000000000000 ) ;
#6932 = VERTEX_POINT ( 'NONE', #560 ) ;
#6933 = VERTEX_POINT ( 'NONE', #6035 ) ;
#6934 = ORIENTED_EDGE ( 'NONE', *, *, #1300, .T. ) ;
#6935 = CARTESIAN_POINT ( 'NONE',  ( 5.000000000000000000, 5.000000000000000000, 7.000000000000006217 ) ) ;
#6936 = CARTESIAN_POINT ( 'NONE',  ( 2.649999999999993694, 157.5000000000000284, 5.000000000000000000 ) ) ;
#6937 = VECTOR ( 'NONE', #5010, 1000.000000000000000 ) ;
#6938 = ADVANCED_FACE ( 'NONE', ( #4737 ), #5988, .T. ) ;
#6939 = EDGE_CURVE ( 'NONE', #6477, #7506, #5475, .T. ) ;
#6940 = ORIENTED_EDGE ( 'NONE', *, *, #1895, .T. ) ;
#6941 = CARTESIAN_POINT ( 'NONE',  ( 20.00000000000000000, 0.000000000000000000, 120.0000000000000142 ) ) ;
#6942 = EDGE_LOOP ( 'NONE', ( #3572, #1545, #2046, #7613 ) ) ;
#6943 = FILL_AREA_STYLE ('',( #4382 ) ) ;
#6944 = CARTESIAN_POINT ( 'NONE',  ( 136.6666666666666288, -14.99999999999999822, 162.5000000000000853 ) ) ;
#6945 = VECTOR ( 'NONE', #7454, 1000.000000000000000 ) ;
#6946 = ITEM_DEFINED_TRANSFORMATION ( 'NONE', 'NONE', #6689,  #594 ) ;
#6947 = ORIENTED_EDGE ( 'NONE', *, *, #2375, .F. ) ;
#6948 = ORIENTED_EDGE ( 'NONE', *, *, #7554, .T. ) ;
#6949 = PLANE ( 'NONE',  #5493 ) ;
#6950 = CARTESIAN_POINT ( 'NONE',  ( 88.00000000000000000, -25.00000000000000000, -124.4814250403154574 ) ) ;
#6951 = DIRECTION ( 'NONE',  ( 0.000000000000000000, 1.000000000000000000, 0.000000000000000000 ) ) ;
#6952 = DIRECTION ( 'NONE',  ( -1.000000000000000000, 0.000000000000000000, 0.000000000000000000 ) ) ;
#6953 = ORIENTED_EDGE ( 'NONE', *, *, #1892, .T. ) ;
#6954 = EDGE_CURVE ( 'NONE', #806, #2406, #1255, .T. ) ;
#6955 = DIRECTION ( 'NONE',  ( 0.000000000000000000, 0.000000000000000000, 1.000000000000000000 ) ) ;
#6956 = CARTESIAN_POINT ( 'NONE',  ( -5.000000000000001776, 5.000000000000001776, 140.0000000000000000 ) ) ;
#6957 = EDGE_LOOP ( 'NONE', ( #415, #6245 ) ) ;
#6958 = ORIENTED_EDGE ( 'NONE', *, *, #6884, .F. ) ;
#6959 = LINE ( 'NONE', #7005, #3659 ) ;
#6960 = CARTESIAN_POINT ( 'NONE',  ( 2.100000000000000089, 0.000000000000000000, -4.694516984716113228 ) ) ;
#6961 = LINE ( 'NONE', #1617, #8308 ) ;
#6962 = AXIS2_PLACEMENT_3D ( 'NONE', #2913, #5561, #960 ) ;
#6963 = FACE_OUTER_BOUND ( 'NONE', #6973, .T. ) ;
#6964 = ORIENTED_EDGE ( 'NONE', *, *, #8543, .F. ) ;
#6965 = LINE ( 'NONE', #4143, #5954 ) ;
#6966 =( NAMED_UNIT ( * ) SI_UNIT ( $, .STERADIAN. ) SOLID_ANGLE_UNIT ( ) );
#6967 = ORIENTED_EDGE ( 'NONE', *, *, #6500, .F. ) ;
#6968 = DIRECTION ( 'NONE',  ( 1.000000000000000000, 0.000000000000000000, 0.000000000000000000 ) ) ;
#6969 = CARTESIAN_POINT ( 'NONE',  ( 5.560781378645575757, 0.000000000000000000, -4.000000000000000000 ) ) ;
#6970 = CARTESIAN_POINT ( 'NONE',  ( 439.9999999999999432, -20.00000000000000000, 16.31857495968447225 ) ) ;
#6971 = CARTESIAN_POINT ( 'NONE',  ( 136.6666666666666288, -20.00000000000000000, 162.5000000000000853 ) ) ;
#6972 = AXIS2_PLACEMENT_3D ( 'NONE', #3738, #1173, #5731 ) ;
#6973 = EDGE_LOOP ( 'NONE', ( #6811, #2618, #619, #2730 ) ) ;
#6974 = VECTOR ( 'NONE', #1466, 1000.000000000000000 ) ;
#6975 = ORIENTED_EDGE ( 'NONE', *, *, #4059, .F. ) ;
#6976 = ORIENTED_EDGE ( 'NONE', *, *, #5474, .T. ) ;
#6977 = VECTOR ( 'NONE', #6624, 1000.000000000000000 ) ;
#6978 = DIRECTION ( 'NONE',  ( 0.000000000000000000, 0.000000000000000000, -1.000000000000000000 ) ) ;
#6979 = LINE ( 'NONE', #5632, #6012 ) ;
#6980 = CIRCLE ( 'NONE', #1285, 2.649999999999985700 ) ;
#6981 = ORIENTED_EDGE ( 'NONE', *, *, #5934, .T. ) ;
#6982 = CARTESIAN_POINT ( 'NONE',  ( -5.000000000000001776, 5.000000000000001776, 148.0000000000000284 ) ) ;
#6983 = AXIS2_PLACEMENT_3D ( 'NONE', #3571, #6219, #8235 ) ;
#6984 = ADVANCED_FACE ( 'NONE', ( #3877 ), #7215, .F. ) ;
#6985 = EDGE_LOOP ( 'NONE', ( #3785, #318 ) ) ;
#6986 =( NAMED_UNIT ( * ) SI_UNIT ( $, .STERADIAN. ) SOLID_ANGLE_UNIT ( ) );
#6987 = DIRECTION ( 'NONE',  ( 0.000000000000000000, 0.000000000000000000, 1.000000000000000000 ) ) ;
#6988 = EDGE_CURVE ( 'NONE', #1439, #54, #7284, .T. ) ;
#6989 = ORIENTED_EDGE ( 'NONE', *, *, #1810, .T. ) ;
#6990 = VECTOR ( 'NONE', #6480, 1000.000000000000000 ) ;
#6991 = ORIENTED_EDGE ( 'NONE', *, *, #6775, .T. ) ;
#6992 = FACE_OUTER_BOUND ( 'NONE', #7054, .T. ) ;
#6993 = ADVANCED_FACE ( 'NONE', ( #8579, #7304 ), #3306, .T. ) ;
#6994 = MECHANICAL_DESIGN_GEOMETRIC_PRESENTATION_REPRESENTATION (  '', ( #33 ), #7706 ) ;
#6995 = DIRECTION ( 'NONE',  ( 1.000000000000000000, 0.000000000000000000, 0.000000000000000000 ) ) ;
#6996 = PRESENTATION_LAYER_ASSIGNMENT (  '', '', ( #4916 ) ) ;
#6997 = CARTESIAN_POINT ( 'NONE',  ( -31.74999999999995737, 0.000000000000000000, 2.500000000000000888 ) ) ;
#6998 = FACE_OUTER_BOUND ( 'NONE', #656, .T. ) ;
#6999 = VERTEX_POINT ( 'NONE', #1388 ) ;
#7000 = VECTOR ( 'NONE', #1637, 1000.000000000000114 ) ;
#7001 = DIRECTION ( 'NONE',  ( 6.123233995736766036E-17, -1.000000000000000000, 0.000000000000000000 ) ) ;
#7002 = FACE_OUTER_BOUND ( 'NONE', #3462, .T. ) ;
#7003 = ORIENTED_EDGE ( 'NONE', *, *, #661, .F. ) ;
#7004 = ORIENTED_EDGE ( 'NONE', *, *, #5602, .F. ) ;
#7005 = CARTESIAN_POINT ( 'NONE',  ( -5.000000000000001776, 5.000000000000001776, 148.0000000000000284 ) ) ;
#7006 = PLANE ( 'NONE',  #3258 ) ;
#7007 = AXIS2_PLACEMENT_3D ( 'NONE', #7671, #6442, #3703 ) ;
#7008 = EDGE_CURVE ( 'NONE', #7420, #7355, #2051, .T. ) ;
#7009 = CARTESIAN_POINT ( 'NONE',  ( 5.000000000000000000, -5.000000000000000000, 148.0000000000000284 ) ) ;
#7010 = DIRECTION ( 'NONE',  ( 0.000000000000000000, -1.000000000000000000, 0.000000000000000000 ) ) ;
#7011 = VERTEX_POINT ( 'NONE', #5387 ) ;
#7012 = CYLINDRICAL_SURFACE ( 'NONE', #8485, 2.500000000000000888 ) ;
#7013 = PRODUCT_CONTEXT ( 'NONE', #3917, 'mechanical' ) ;
#7014 = ORIENTED_EDGE ( 'NONE', *, *, #4844, .T. ) ;
#7015 = CARTESIAN_POINT ( 'NONE',  ( -30.00000000000000000, -15.00000000000000000, 140.0000000000000000 ) ) ;
#7016 = DIRECTION ( 'NONE',  ( -0.000000000000000000, 1.000000000000000000, -0.000000000000000000 ) ) ;
#7017 = EDGE_CURVE ( 'NONE', #2221, #848, #4784, .T. ) ;
#7018 = ADVANCED_FACE ( 'NONE', ( #4693 ), #3916, .F. ) ;
#7019 = CARTESIAN_POINT ( 'NONE',  ( 0.000000000000000000, 0.000000000000000000, -63.99999999999997158 ) ) ;
#7020 = ADVANCED_FACE ( 'NONE', ( #7351 ), #1340, .F. ) ;
#7021 = DIRECTION ( 'NONE',  ( -0.000000000000000000, -0.000000000000000000, -1.000000000000000000 ) ) ;
#7022 = CARTESIAN_POINT ( 'NONE',  ( -4.000000000000000000, -1.680117682357936904, -3.316611593218794951 ) ) ;
#7023 = ORIENTED_EDGE ( 'NONE', *, *, #2666, .T. ) ;
#7024 = EDGE_LOOP ( 'NONE', ( #4584, #6677 ) ) ;
#7025 = CARTESIAN_POINT ( 'NONE',  ( -1.240299975428134203E-15, -4.736529461165891242, -3.681130640444276292 ) ) ;
#7026 = VECTOR ( 'NONE', #3731, 1000.000000000000000 ) ;
#7027 = FACE_BOUND ( 'NONE', #6164, .T. ) ;
#7028 = APPLICATION_CONTEXT ( 'automotive_design' ) ;
#7029 = ORIENTED_EDGE ( 'NONE', *, *, #4759, .F. ) ;
#7030 = AXIS2_PLACEMENT_3D ( 'NONE', #3997, #8048, #1993 ) ;
#7031 = LINE ( 'NONE', #3035, #2176 ) ;
#7032 = ORIENTED_EDGE ( 'NONE', *, *, #4396, .T. ) ;
#7033 = LINE ( 'NONE', #8181, #924 ) ;
#7034 = CONTEXT_DEPENDENT_SHAPE_REPRESENTATION ( #2434, #5586 ) ;
#7035 = ORIENTED_EDGE ( 'NONE', *, *, #3491, .T. ) ;
#7036 = ORIENTED_EDGE ( 'NONE', *, *, #6503, .F. ) ;
#7037 = CARTESIAN_POINT ( 'NONE',  ( 0.000000000000000000, 0.000000000000000000, -135.0000000000000000 ) ) ;
#7038 = DIRECTION ( 'NONE',  ( 1.000000000000000000, 0.000000000000000000, 0.000000000000000000 ) ) ;
#7039 = AXIS2_PLACEMENT_3D ( 'NONE', #8477, #8396, #2438 ) ;
#7040 = CIRCLE ( 'NONE', #4527, 20.00000000000000000 ) ;
#7041 = DIRECTION ( 'NONE',  ( -1.000000000000000000, -0.000000000000000000, -0.000000000000000000 ) ) ;
#7042 = LINE ( 'NONE', #5884, #682 ) ;
#7043 = ORIENTED_EDGE ( 'NONE', *, *, #378, .T. ) ;
#7044 = EDGE_CURVE ( 'NONE', #3680, #7903, #6647, .T. ) ;
#7045 = VECTOR ( 'NONE', #8241, 1000.000000000000000 ) ;
#7046 = DIRECTION ( 'NONE',  ( 0.000000000000000000, 0.000000000000000000, 1.000000000000000000 ) ) ;
#7047 = DIRECTION ( 'NONE',  ( -0.000000000000000000, 1.000000000000000000, -0.000000000000000000 ) ) ;
#7048 = VERTEX_POINT ( 'NONE', #3351 ) ;
#7049 = VERTEX_POINT ( 'NONE', #5860 ) ;
#7050 = LINE ( 'NONE', #4964, #28 ) ;
#7051 = LINE ( 'NONE', #4400, #7154 ) ;
#7052 = LINE ( 'NONE', #1095, #3701 ) ;
#7053 = DIRECTION ( 'NONE',  ( 0.000000000000000000, 0.000000000000000000, -1.000000000000000000 ) ) ;
#7054 = EDGE_LOOP ( 'NONE', ( #6296, #7072 ) ) ;
#7055 = VECTOR ( 'NONE', #8149, 1000.000000000000000 ) ;
#7056 = VERTEX_POINT ( 'NONE', #26 ) ;
#7057 = PRODUCT_DEFINITION_SHAPE ( 'NONE', 'NONE',  #8622 ) ;
#7058 = DIRECTION ( 'NONE',  ( 1.000000000000000000, 0.000000000000000000, 0.000000000000000000 ) ) ;
#7059 = DIRECTION ( 'NONE',  ( -1.000000000000000000, 0.000000000000000000, 0.000000000000000000 ) ) ;
#7060 = LINE ( 'NONE', #5669, #7509 ) ;
#7061 = CARTESIAN_POINT ( 'NONE',  ( 5.000000000000000000, -5.000000000000000000, 148.0000000000000284 ) ) ;
#7062 = FACE_OUTER_BOUND ( 'NONE', #658, .T. ) ;
#7063 = VERTEX_POINT ( 'NONE', #2701 ) ;
#7064 = EDGE_CURVE ( 'NONE', #54, #1439, #3959, .T. ) ;
#7065 = AXIS2_PLACEMENT_3D ( 'NONE', #5440, #4272, #6881 ) ;
#7066 = FACE_OUTER_BOUND ( 'NONE', #7159, .T. ) ;
#7067 = EDGE_CURVE ( 'NONE', #2451, #1549, #245, .T. ) ;
#7068 = PLANE ( 'NONE',  #2729 ) ;
#7069 = DIRECTION ( 'NONE',  ( -0.000000000000000000, -0.000000000000000000, 1.000000000000000000 ) ) ;
#7070 = CARTESIAN_POINT ( 'NONE',  ( -20.00000000000000000, 2.449293598294706513E-15, 27.00000000000001066 ) ) ;
#7071 = UNCERTAINTY_MEASURE_WITH_UNIT (LENGTH_MEASURE( 1.000000000000000082E-05 ), #743, 'distance_accuracy_value', 'NONE');
#7072 = ORIENTED_EDGE ( 'NONE', *, *, #6443, .T. ) ;
#7073 = CARTESIAN_POINT ( 'NONE',  ( -10.00000000000000000, 1.224646799147353256E-15, 140.0000000000000000 ) ) ;
#7074 = VERTEX_POINT ( 'NONE', #4091 ) ;
#7075 = DIRECTION ( 'NONE',  ( -0.000000000000000000, -0.000000000000000000, 1.000000000000000000 ) ) ;
#7076 = CONTEXT_DEPENDENT_SHAPE_REPRESENTATION ( #802, #7057 ) ;
#7077 = ORIENTED_EDGE ( 'NONE', *, *, #1575, .T. ) ;
#7078 = ORIENTED_EDGE ( 'NONE', *, *, #3832, .T. ) ;
#7079 = LINE ( 'NONE', #1124, #171 ) ;
#7080 = VECTOR ( 'NONE', #2466, 1000.000000000000000 ) ;
#7081 = CARTESIAN_POINT ( 'NONE',  ( 303.3333333333333144, -25.00000000000000000, 162.5000000000000853 ) ) ;
#7082 = DIRECTION ( 'NONE',  ( 0.000000000000000000, -1.000000000000000000, 0.000000000000000000 ) ) ;
#7083 = CIRCLE ( 'NONE', #3337, 5.560781378645573980 ) ;
#7084 = ORIENTED_EDGE ( 'NONE', *, *, #2112, .T. ) ;
#7085 = CARTESIAN_POINT ( 'NONE',  ( 219.9999999999999716, -30.00000000000000355, 162.5000000000000853 ) ) ;
#7086 = CARTESIAN_POINT ( 'NONE',  ( 0.000000000000000000, 0.000000000000000000, -97.99999999999997158 ) ) ;
#7087 = ORIENTED_EDGE ( 'NONE', *, *, #175, .F. ) ;
#7088 = ORIENTED_EDGE ( 'NONE', *, *, #6884, .T. ) ;
#7089 = FACE_OUTER_BOUND ( 'NONE', #5138, .T. ) ;
#7090 = CARTESIAN_POINT ( 'NONE',  ( 2.500000000000000444, 0.000000000000000000, -25.03750572909317285 ) ) ;
#7091 = AXIS2_PLACEMENT_3D ( 'NONE', #8338, #7683, #3739 ) ;
#7092 = CARTESIAN_POINT ( 'NONE',  ( 0.000000000000000000, 0.000000000000000000, 42.00000000000000711 ) ) ;
#7093 = PLANE ( 'NONE',  #2498 ) ;
#7094 =( BOUNDED_SURFACE ( )  B_SPLINE_SURFACE ( 3, 2, ( 
 ( #8188, #1474, #4913 ),
 ( #4171, #154, #6912 ),
 ( #7526, #3483, #3440 ),
 ( #6257, #2870, #5390 ),
 ( #2220, #4871, #1564 ),
 ( #913, #3567, #6216 ) ),
 .UNSPECIFIED., .F., .F., .F. ) 
 B_SPLINE_SURFACE_WITH_KNOTS ( ( 4, 2, 4 ),
 ( 3, 3 ),
 ( 0.02032853247518126918, 0.02278863295364821906, 0.02524873343211517240 ),
 ( 0.000000000000000000, 1.000000000000000000 ),
 .UNSPECIFIED. ) 
 GEOMETRIC_REPRESENTATION_ITEM ( )  RATIONAL_B_SPLINE_SURFACE ( (
 ( 1.000000000000000000, 0.8047781615896837382, 1.000000000000000000),
 ( 1.000000000000000000, 0.8123767586289252218, 1.000000000000000000),
 ( 1.000000000000000000, 0.8190662415564388121, 1.000000000000000000),
 ( 1.000000000000000000, 0.8192361015669026303, 1.000000000000000000),
 ( 1.000000000000000000, 0.8126135807103900266, 1.000000000000000000),
 ( 1.000000000000000000, 0.8047712338318593339, 1.000000000000000000) ) ) 
 REPRESENTATION_ITEM ( '' )  SURFACE ( )  );
#7095 = ORIENTED_EDGE ( 'NONE', *, *, #1093, .F. ) ;
#7096 = EDGE_CURVE ( 'NONE', #6261, #3580, #4233, .T. ) ;
#7097 = VERTEX_POINT ( 'NONE', #2217 ) ;
#7098 = FACE_OUTER_BOUND ( 'NONE', #5350, .T. ) ;
#7099 = EDGE_CURVE ( 'NONE', #1917, #3262, #6778, .T. ) ;
#7100 = B_SPLINE_CURVE_WITH_KNOTS ( 'NONE', 3,
 ( #5517, #2218, #4259, #6911, #956, #3607, #4131, #4870 ),
 .UNSPECIFIED., .F., .F.,
 ( 4, 2, 2, 4 ),
 ( 0.000000000000000000, 0.002450665683189818828, 0.003675998524784728459, 0.004901331366379638524 ),
 .UNSPECIFIED. ) ;
#7101 = DIRECTION ( 'NONE',  ( 0.000000000000000000, 0.000000000000000000, -1.000000000000000000 ) ) ;
#7102 = DIRECTION ( 'NONE',  ( -0.000000000000000000, 0.000000000000000000, -1.000000000000000000 ) ) ;
#7103 = CARTESIAN_POINT ( 'NONE',  ( 10.00000000000000000, 0.000000000000000000, -135.0000000000000000 ) ) ;
#7104 = FILL_AREA_STYLE ('',( #1062 ) ) ;
#7105 = ORIENTED_EDGE ( 'NONE', *, *, #7723, .T. ) ;
#7106 = PRESENTATION_STYLE_ASSIGNMENT (( #4455 ) ) ;
#7107 = PLANE ( 'NONE',  #8273 ) ;
#7108 = DIRECTION ( 'NONE',  ( 0.000000000000000000, 0.000000000000000000, 1.000000000000000000 ) ) ;
#7109 = ADVANCED_FACE ( 'NONE', ( #1561 ), #1595, .T. ) ;
#7110 = PRODUCT_DEFINITION_FORMATION_WITH_SPECIFIED_SOURCE ( 'ANY', '', #8034, .NOT_KNOWN. ) ;
#7111 = VECTOR ( 'NONE', #3431, 1000.000000000000000 ) ;
#7112 = CARTESIAN_POINT ( 'NONE',  ( 2.500000000000000000, 0.000000000000000000, 0.000000000000000000 ) ) ;
#7113 = ORIENTED_EDGE ( 'NONE', *, *, #3133, .T. ) ;
#7114 = FILL_AREA_STYLE ('',( #4585 ) ) ;
#7115 = ADVANCED_FACE ( 'NONE', ( #7435 ), #4953, .T. ) ;
#7116 = VECTOR ( 'NONE', #843, 1000.000000000000000 ) ;
#7117 = CARTESIAN_POINT ( 'NONE',  ( 5.000000000000000000, 5.000000000000000000, -63.99999999999997158 ) ) ;
#7118 = ITEM_DEFINED_TRANSFORMATION ( 'NONE', 'NONE', #4891,  #594 ) ;
#7119 = ORIENTED_EDGE ( 'NONE', *, *, #30, .F. ) ;
#7120 = ORIENTED_EDGE ( 'NONE', *, *, #7318, .F. ) ;
#7121 = ORIENTED_EDGE ( 'NONE', *, *, #3295, .T. ) ;
#7122 = FACE_OUTER_BOUND ( 'NONE', #5248, .T. ) ;
#7123 = CIRCLE ( 'NONE', #3368, 10.00000000000000000 ) ;
#7124 = DIRECTION ( 'NONE',  ( -0.000000000000000000, -0.000000000000000000, 1.000000000000000000 ) ) ;
#7125 = CIRCLE ( 'NONE', #4900, 2.500000000000000888 ) ;
#7126 = EDGE_CURVE ( 'NONE', #8255, #730, #955, .T. ) ;
#7127 = LINE ( 'NONE', #473, #3145 ) ;
#7128 = ORIENTED_EDGE ( 'NONE', *, *, #8436, .T. ) ;
#7129 = AXIS2_PLACEMENT_3D ( 'NONE', #3876, #2612, #3915 ) ;
#7130 = DIRECTION ( 'NONE',  ( 1.000000000000000000, 6.123233995736766036E-17, -6.123233995736764803E-17 ) ) ;
#7131 = DIRECTION ( 'NONE',  ( -1.000000000000000000, 0.000000000000000000, -0.000000000000000000 ) ) ;
#7132 = ORIENTED_EDGE ( 'NONE', *, *, #8064, .T. ) ;
#7133 = VECTOR ( 'NONE', #5034, 1000.000000000000000 ) ;
#7134 = ORIENTED_EDGE ( 'NONE', *, *, #3203, .T. ) ;
#7135 = CIRCLE ( 'NONE', #5735, 2.649999999999985700 ) ;
#7136 = DIRECTION ( 'NONE',  ( -1.734723475976807587E-16, 1.000000000000000000, 0.000000000000000000 ) ) ;
#7137 = PLANE ( 'NONE',  #331 ) ;
#7138 = AXIS2_PLACEMENT_3D ( 'NONE', #5374, #8046, #2077 ) ;
#7139 = STYLED_ITEM ( 'NONE', ( #5277 ), #7622 ) ;
#7140 = LINE ( 'NONE', #3837, #7594 ) ;
#7141 = FACE_OUTER_BOUND ( 'NONE', #5453, .T. ) ;
#7142 = ORIENTED_EDGE ( 'NONE', *, *, #5176, .F. ) ;
#7143 = ORIENTED_EDGE ( 'NONE', *, *, #2741, .T. ) ;
#7144 = ORIENTED_EDGE ( 'NONE', *, *, #6103, .F. ) ;
#7145 = CARTESIAN_POINT ( 'NONE',  ( 2.500000000000000000, 1.178949249685213863, -2.042000000000001148 ) ) ;
#7146 = EDGE_CURVE ( 'NONE', #4010, #1033, #4930, .T. ) ;
#7147 = AXIS2_PLACEMENT_3D ( 'NONE', #8508, #4535, #7194 ) ;
#7148 = ADVANCED_FACE ( 'NONE', ( #911 ), #4256, .F. ) ;
#7149 = FACE_BOUND ( 'NONE', #5278, .T. ) ;
#7150 = CARTESIAN_POINT ( 'NONE',  ( 439.9999999999999432, -25.00000000000000000, 18.96857495968446017 ) ) ;
#7151 = ADVANCED_FACE ( 'NONE', ( #2950 ), #4868, .F. ) ;
#7152 = DIRECTION ( 'NONE',  ( 1.000000000000000000, 0.000000000000000000, 0.000000000000000000 ) ) ;
#7153 = FILL_AREA_STYLE_COLOUR ( '', #946 ) ;
#7154 = VECTOR ( 'NONE', #7717, 1000.000000000000000 ) ;
#7155 = EDGE_CURVE ( 'NONE', #8492, #2732, #2823, .T. ) ;
#7156 = DIRECTION ( 'NONE',  ( 1.000000000000000000, 0.000000000000000000, 0.000000000000000000 ) ) ;
#7157 = DIRECTION ( 'NONE',  ( -0.000000000000000000, 1.000000000000000000, -0.000000000000000000 ) ) ;
#7158 = CARTESIAN_POINT ( 'NONE',  ( 170.9999999999999716, -4.999999999999998224, 145.0000000000000284 ) ) ;
#7159 = EDGE_LOOP ( 'NONE', ( #5377, #3787, #7929, #2107 ) ) ;
#7160 = FILL_AREA_STYLE ('',( #7199 ) ) ;
#7161 = CYLINDRICAL_SURFACE ( 'NONE', #4264, 2.649999999999985700 ) ;
#7162 = ORIENTED_EDGE ( 'NONE', *, *, #6279, .F. ) ;
#7163 = DIRECTION ( 'NONE',  ( 0.000000000000000000, 0.000000000000000000, -1.000000000000000000 ) ) ;
#7164 = CARTESIAN_POINT ( 'NONE',  ( 2.000000000000008882, 3.464101615137749945, 0.000000000000000000 ) ) ;
#7165 = AXIS2_PLACEMENT_3D ( 'NONE', #995, #5428, #5558 ) ;
#7166 = DIRECTION ( 'NONE',  ( 0.000000000000000000, -0.000000000000000000, -1.000000000000000000 ) ) ;
#7167 = ORIENTED_EDGE ( 'NONE', *, *, #1149, .F. ) ;
#7168 = DIRECTION ( 'NONE',  ( 0.000000000000000000, 0.000000000000000000, 1.000000000000000000 ) ) ;
#7169 = APPLICATION_PROTOCOL_DEFINITION ( 'draft international standard', 'automotive_design', 1998, #5844 ) ;
#7170 = DIRECTION ( 'NONE',  ( -1.000000000000000000, 0.000000000000000000, 0.000000000000000000 ) ) ;
#7171 = EDGE_LOOP ( 'NONE', ( #5887, #5901, #6940, #5095 ) ) ;
#7172 = ORIENTED_EDGE ( 'NONE', *, *, #30, .T. ) ;
#7173 = AXIS2_PLACEMENT_3D ( 'NONE', #772, #278, #8136 ) ;
#7174 = EDGE_CURVE ( 'NONE', #1258, #1044, #6352, .T. ) ;
#7176 = CIRCLE ( 'NONE', #1065, 10.00000000000000000 ) ;
#7175 = LINE ( 'NONE', #5171, #1721 ) ;
#7177 = EDGE_CURVE ( 'NONE', #3488, #1501, #5557, .T. ) ;
#7178 = CARTESIAN_POINT ( 'NONE',  ( -5.000000000000001776, 5.000000000000001776, -0.9999999999999940048 ) ) ;
#7179 = EDGE_CURVE ( 'NONE', #3708, #7568, #199, .T. ) ;
#7180 =( GEOMETRIC_REPRESENTATION_CONTEXT ( 3 ) GLOBAL_UNCERTAINTY_ASSIGNED_CONTEXT ( ( #2945 ) ) GLOBAL_UNIT_ASSIGNED_CONTEXT ( ( #2390, #5026, #7817 ) ) REPRESENTATION_CONTEXT ( 'NONE', 'WORKASPACE' ) );
#7181 = CARTESIAN_POINT ( 'NONE',  ( 5.000000000000000888, 0.000000000000000000, 0.000000000000000000 ) ) ;
#7182 = AXIS2_PLACEMENT_3D ( 'NONE', #4544, #7200, #1239 ) ;
#7183 = PRODUCT_DEFINITION_SHAPE ( 'NONE', 'NONE',  #8616 ) ;
#7184 = CARTESIAN_POINT ( 'NONE',  ( 2.500000000000000000, 0.000000000000000000, 0.000000000000000000 ) ) ;
#7185 = EDGE_LOOP ( 'NONE', ( #5239, #6079 ) ) ;
#7186 = VERTEX_POINT ( 'NONE', #3520 ) ;
#7187 = DIRECTION ( 'NONE',  ( -0.000000000000000000, 1.000000000000000000, -0.000000000000000000 ) ) ;
#7188 = DIRECTION ( 'NONE',  ( -1.000000000000000000, 1.734723475976807341E-16, -0.000000000000000000 ) ) ;
#7189 = CARTESIAN_POINT ( 'NONE',  ( 0.000000000000000000, 0.000000000000000000, -63.99999999999997158 ) ) ;
#7190 = CARTESIAN_POINT ( 'NONE',  ( -5.000000000000001776, 5.000000000000001776, 148.0000000000000284 ) ) ;
#7191 =( REPRESENTATION_RELATIONSHIP ('NONE','NONE', #3312, #1479 ) REPRESENTATION_RELATIONSHIP_WITH_TRANSFORMATION ( #2253 )SHAPE_REPRESENTATION_RELATIONSHIP( ) );
#7192 = SURFACE_SIDE_STYLE ('',( #5189 ) ) ;
#7193 = PLANE ( 'NONE',  #5857 ) ;
#7194 = DIRECTION ( 'NONE',  ( 1.000000000000000000, 0.000000000000000000, 0.000000000000000000 ) ) ;
#7195 = DIRECTION ( 'NONE',  ( 1.000000000000000000, 0.000000000000000000, 0.000000000000000000 ) ) ;
#7196 = CARTESIAN_POINT ( 'NONE',  ( -5.000000000000000000, -5.000000000000000000, 148.0000000000000284 ) ) ;
#7197 = CARTESIAN_POINT ( 'NONE',  ( 2.500000000000000000, -2.357898499370432610, 3.252606517456513302E-15 ) ) ;
#7198 = ORIENTED_EDGE ( 'NONE', *, *, #8059, .T. ) ;
#7199 = FILL_AREA_STYLE_COLOUR ( '', #2137 ) ;
#7200 = DIRECTION ( 'NONE',  ( -0.000000000000000000, 1.471414886128461471E-15, 1.000000000000000000 ) ) ;
#7201 = ORIENTED_EDGE ( 'NONE', *, *, #5459, .F. ) ;
#7202 = DIRECTION ( 'NONE',  ( -0.000000000000000000, -0.000000000000000000, 1.000000000000000000 ) ) ;
#7203 = LINE ( 'NONE', #4592, #6571 ) ;
#7204 = AXIS2_PLACEMENT_3D ( 'NONE', #2402, #2705, #5300 ) ;
#7205 = EDGE_CURVE ( 'NONE', #1044, #3371, #5924, .T. ) ;
#7206 = CARTESIAN_POINT ( 'NONE',  ( -5.000000000000000000, -5.000000000000000000, 148.0000000000000284 ) ) ;
#7207 = ORIENTED_EDGE ( 'NONE', *, *, #4793, .F. ) ;
#7208 = DIRECTION ( 'NONE',  ( -1.000000000000000000, 0.000000000000000000, 0.000000000000000000 ) ) ;
#7209 = AXIS2_PLACEMENT_3D ( 'NONE', #7184, #3226, #4740 ) ;
#7210 =( NAMED_UNIT ( * ) PLANE_ANGLE_UNIT ( ) SI_UNIT ( $, .RADIAN. ) );
#7211 = CARTESIAN_POINT ( 'NONE',  ( 0.000000000000000000, 0.000000000000000000, -120.5685424949237898 ) ) ;
#7212 = ORIENTED_EDGE ( 'NONE', *, *, #4173, .F. ) ;
#7213 = VERTEX_POINT ( 'NONE', #289 ) ;
#7214 = DIRECTION ( 'NONE',  ( 0.000000000000000000, 0.000000000000000000, -1.000000000000000000 ) ) ;
#7215 = PLANE ( 'NONE',  #7989 ) ;
#7216 = VECTOR ( 'NONE', #42, 1000.000000000000000 ) ;
#7217 = CARTESIAN_POINT ( 'NONE',  ( -2.688821387764050996E-14, -4.618802153517012954, -0.4999999999999995559 ) ) ;
#7218 = EDGE_CURVE ( 'NONE', #6599, #1013, #2782, .T. ) ;
#7219 = CARTESIAN_POINT ( 'NONE',  ( 269.0000000000000000, 5.000000000000000000, 145.0000000000000284 ) ) ;
#7220 = VERTEX_POINT ( 'NONE', #6167 ) ;
#7221 = ORIENTED_EDGE ( 'NONE', *, *, #6348, .T. ) ;
#7222 = LINE ( 'NONE', #659, #4210 ) ;
#7223 = DIRECTION ( 'NONE',  ( -1.000000000000000000, 1.734723475976807341E-16, -0.000000000000000000 ) ) ;
#7224 = CARTESIAN_POINT ( 'NONE',  ( 0.000000000000000000, 0.000000000000000000, 62.00000000000001421 ) ) ;
#7225 = ORIENTED_EDGE ( 'NONE', *, *, #299, .F. ) ;
#7226 = VECTOR ( 'NONE', #3169, 1000.000000000000000 ) ;
#7227 = CARTESIAN_POINT ( 'NONE',  ( -4.999999999999998224, 5.000000000000001776, 145.0000000000000284 ) ) ;
#7228 = DIRECTION ( 'NONE',  ( 0.000000000000000000, 0.000000000000000000, 1.000000000000000000 ) ) ;
#7229 = PRODUCT_DEFINITION ( 'UNKNOWN', '', #6129, #7244 ) ;
#7230 = CARTESIAN_POINT ( 'NONE',  ( -20.00000000000000000, 2.449293598294706513E-15, 120.0000000000000142 ) ) ;
#7231 = LINE ( 'NONE', #6535, #8127 ) ;
#7232 = DIRECTION ( 'NONE',  ( 0.000000000000000000, -0.000000000000000000, 1.000000000000000000 ) ) ;
#7233 = CYLINDRICAL_SURFACE ( 'NONE', #7788, 2.649999999999985700 ) ;
#7234 = CARTESIAN_POINT ( 'NONE',  ( -6.259644161404860030E-16, -4.618802153517027165, -3.433295621305388234 ) ) ;
#7235 = DIRECTION ( 'NONE',  ( -1.000000000000000000, 0.000000000000000000, 0.000000000000000000 ) ) ;
#7236 = MECHANICAL_DESIGN_GEOMETRIC_PRESENTATION_REPRESENTATION (  '', ( #5986 ), #434 ) ;
#7237 = ORIENTED_EDGE ( 'NONE', *, *, #1380, .F. ) ;
#7238 = LINE ( 'NONE', #5803, #6620 ) ;
#7239 = CONTEXT_DEPENDENT_SHAPE_REPRESENTATION ( #1357, #1639 ) ;
#7240 = ORIENTED_EDGE ( 'NONE', *, *, #6829, .T. ) ;
#7241 = CARTESIAN_POINT ( 'NONE',  ( 136.6666666666666288, -20.00000000000000000, 162.5000000000000853 ) ) ;
#7242 = DIRECTION ( 'NONE',  ( 0.000000000000000000, 0.000000000000000000, 1.000000000000000000 ) ) ;
#7243 = AXIS2_PLACEMENT_3D ( 'NONE', #2693, #2570, #3390 ) ;
#7244 = PRODUCT_DEFINITION_CONTEXT ( 'detailed design', #6861, 'design' ) ;
#7245 = AXIS2_PLACEMENT_3D ( 'NONE', #8507, #1896, #7566 ) ;
#7246 = EDGE_CURVE ( 'NONE', #5548, #5730, #8317, .T. ) ;
#7247 = CARTESIAN_POINT ( 'NONE',  ( -5.000000000000001776, 5.000000000000001776, 148.0000000000000284 ) ) ;
#7248 = EDGE_CURVE ( 'NONE', #2875, #2638, #3130, .T. ) ;
#7249 = ORIENTED_EDGE ( 'NONE', *, *, #8202, .T. ) ;
#7250 = CARTESIAN_POINT ( 'NONE',  ( 303.3333333333333144, -14.99999999999999822, 159.8500000000001080 ) ) ;
#7251 = APPLICATION_PROTOCOL_DEFINITION ( 'draft international standard', 'automotive_design', 1998, #6576 ) ;
#7252 = CARTESIAN_POINT ( 'NONE',  ( 5.000000000000000000, -5.000000000000000000, 140.0000000000000000 ) ) ;
#7253 = EDGE_LOOP ( 'NONE', ( #5131, #2308, #4804, #5076 ) ) ;
#7254 = VECTOR ( 'NONE', #5260, 1000.000000000000000 ) ;
#7255 = ADVANCED_FACE ( 'NONE', ( #4301 ), #7616, .T. ) ;
#7256 = B_SPLINE_CURVE_WITH_KNOTS ( 'NONE', 3,
 ( #4600, #5903, #3220, #7258, #4646 ),
 .UNSPECIFIED., .F., .F.,
 ( 4, 1, 4 ),
 ( 0.000000000000000000, 0.002309401076758505790, 0.004618802153517011580 ),
 .UNSPECIFIED. ) ;
#7257 = ORIENTED_EDGE ( 'NONE', *, *, #6214, .F. ) ;
#7258 = CARTESIAN_POINT ( 'NONE',  ( -4.000000000000000888, -1.539600717839011201, -3.300726591567081591 ) ) ;
#7259 = DIRECTION ( 'NONE',  ( -1.000000000000000000, -0.000000000000000000, -0.000000000000000000 ) ) ;
#7260 = VECTOR ( 'NONE', #707, 1000.000000000000000 ) ;
#7261 = CIRCLE ( 'NONE', #4906, 4.250000000000000000 ) ;
#7262 = CARTESIAN_POINT ( 'NONE',  ( 5.000000000000001776, -4.999999999999998224, 139.9990000000000236 ) ) ;
#7263 = DIRECTION ( 'NONE',  ( 0.000000000000000000, 0.000000000000000000, 1.000000000000000000 ) ) ;
#7264 = ORIENTED_EDGE ( 'NONE', *, *, #5836, .F. ) ;
#7265 = VECTOR ( 'NONE', #6784, 1000.000000000000000 ) ;
#7266 = SHAPE_REPRESENTATION_RELATIONSHIP ( 'NONE' , 'NONE' ,  #7424, #6254 ) ;
#7267 = ORIENTED_EDGE ( 'NONE', *, *, #6919, .T. ) ;
#7268 = VECTOR ( 'NONE', #4212, 1000.000000000000000 ) ;
#7269 = DIRECTION ( 'NONE',  ( 0.000000000000000000, 1.000000000000000000, 0.000000000000000000 ) ) ;
#7270 = VECTOR ( 'NONE', #3138, 1000.000000000000000 ) ;
#7271 = EDGE_CURVE ( 'NONE', #7074, #5979, #7977, .T. ) ;
#7272=STYLED_ITEM('',(#8657),#7589);
#7273 = FACE_OUTER_BOUND ( 'NONE', #4898, .T. ) ;
#7274 = DIRECTION ( 'NONE',  ( -1.734723475976806848E-16, -1.000000000000000000, 0.000000000000000000 ) ) ;
#7275 = VERTEX_POINT ( 'NONE', #994 ) ;
#7276 = DIRECTION ( 'NONE',  ( 1.000000000000000000, 0.000000000000000000, 0.000000000000000000 ) ) ;
#7277 = VECTOR ( 'NONE', #896, 1000.000000000000000 ) ;
#7278 = LINE ( 'NONE', #5313, #2260 ) ;
#7279 = CARTESIAN_POINT ( 'NONE',  ( 0.000000000000000000, 0.000000000000000000, -27.99999999999999645 ) ) ;
#7280 = EDGE_CURVE ( 'NONE', #1907, #4164, #8483, .T. ) ;
#7281 = EDGE_CURVE ( 'NONE', #4658, #958, #5687, .T. ) ;
#7282 = CARTESIAN_POINT ( 'NONE',  ( 4.101954839143059139, -2.368264730582948285, -3.681130640444269631 ) ) ;
#7283 = EDGE_CURVE ( 'NONE', #8085, #8486, #1166, .T. ) ;
#7284 = CIRCLE ( 'NONE', #8548, 2.649999999999985700 ) ;
#7285 = DIRECTION ( 'NONE',  ( 0.8191520442889875797, 0.000000000000000000, 0.5735764363510522656 ) ) ;
#7286 = LINE ( 'NONE', #3984, #7353 ) ;
#7287 = CARTESIAN_POINT ( 'NONE',  ( -5.000000000000000000, -5.000000000000000000, 148.0000000000000284 ) ) ;
#7288 = ORIENTED_EDGE ( 'NONE', *, *, #2396, .T. ) ;
#7289 =( NAMED_UNIT ( * ) PLANE_ANGLE_UNIT ( ) SI_UNIT ( $, .RADIAN. ) );
#7290 = VERTEX_POINT ( 'NONE', #3776 ) ;
#7291 = EDGE_CURVE ( 'NONE', #732, #2207, #1651, .T. ) ;
#7292 = EDGE_LOOP ( 'NONE', ( #969, #8461, #292, #1283 ) ) ;
#7293 = PLANE ( 'NONE',  #6877 ) ;
#7294 = DIRECTION ( 'NONE',  ( -0.000000000000000000, -0.000000000000000000, 1.000000000000000000 ) ) ;
#7295 = DIRECTION ( 'NONE',  ( 1.000000000000000000, 0.000000000000000000, 0.000000000000000000 ) ) ;
#7296 = ORIENTED_EDGE ( 'NONE', *, *, #7720, .T. ) ;
#7297 = DIRECTION ( 'NONE',  ( -0.000000000000000000, -0.000000000000000000, 1.000000000000000000 ) ) ;
#7298 = LINE ( 'NONE', #775, #3846 ) ;
#7299 = DIRECTION ( 'NONE',  ( 0.1884548733085491257, -5.551115123125782702E-17, 0.9820818503191367510 ) ) ;
#7300 = CARTESIAN_POINT ( 'NONE',  ( -1.312671235360383548, -3.860931062424228788, -0.05923475698271369466 ) ) ;
#7301 = ORIENTED_EDGE ( 'NONE', *, *, #4099, .T. ) ;
#7302 = ORIENTED_EDGE ( 'NONE', *, *, #5807, .F. ) ;
#7303 = CARTESIAN_POINT ( 'NONE',  ( 5.000000000000000000, -5.000000000000000000, -105.9999999999999858 ) ) ;
#7304 = FACE_OUTER_BOUND ( 'NONE', #8148, .T. ) ;
#7305 = VECTOR ( 'NONE', #7828, 1000.000000000000000 ) ;
#7306 = CLOSED_SHELL ( 'NONE', ( #8542, #4940, #5334, #4014, #932, #6171, #8283, #1615, #2658, #8032, #2334, #567, #4332, #7365, #1812, #4066, #7018, #643, #710, #6126 ) ) ;
#7307 = EDGE_CURVE ( 'NONE', #1599, #2805, #470, .T. ) ;
#7308 = CARTESIAN_POINT ( 'NONE',  ( 4.211405965630455661, 2.460463115436283932, -3.751298928144577882 ) ) ;
#7309 = FACE_OUTER_BOUND ( 'NONE', #8355, .T. ) ;
#7310 = ORIENTED_EDGE ( 'NONE', *, *, #4499, .T. ) ;
#7311 = VECTOR ( 'NONE', #4945, 1000.000000000000000 ) ;
#7312 = CLOSED_SHELL ( 'NONE', ( #4129, #7895, #597, #4169, #3836, #5760, #5965, #5628, #1859, #5967, #1148, #2692, #6155, #1618, #1491, #501, #3770, #8176, #5100, #629, #8299, #5208, #5139, #4738, #1200, #3673, #4018 ) ) ;
#7313 = VERTEX_POINT ( 'NONE', #6950 ) ;
#7314 = DIRECTION ( 'NONE',  ( 0.000000000000000000, 0.000000000000000000, 1.000000000000000000 ) ) ;
#7315 = EDGE_CURVE ( 'NONE', #6262, #8169, #4341, .T. ) ;
#7316 = VECTOR ( 'NONE', #324, 1000.000000000000000 ) ;
#7317 = AXIS2_PLACEMENT_3D ( 'NONE', #5509, #2209, #4206 ) ;
#7318 = EDGE_CURVE ( 'NONE', #5694, #238, #3045, .T. ) ;
#7319 = DIRECTION ( 'NONE',  ( 0.000000000000000000, 0.8660254037844380415, -0.5000000000000012212 ) ) ;
#7320 = DIRECTION ( 'NONE',  ( 0.000000000000000000, 0.000000000000000000, -1.000000000000000000 ) ) ;
#7321 = ORIENTED_EDGE ( 'NONE', *, *, #2742, .T. ) ;
#7322 = DIRECTION ( 'NONE',  ( -0.000000000000000000, -0.000000000000000000, 1.000000000000000000 ) ) ;
#7323 = CIRCLE ( 'NONE', #5792, 10.00000000000000000 ) ;
#7324 = VECTOR ( 'NONE', #617, 1000.000000000000000 ) ;
#7325 = PRODUCT_DEFINITION_SHAPE ( 'NONE', 'NONE',  #8603 ) ;
#7326 = DIRECTION ( 'NONE',  ( 0.000000000000000000, 1.000000000000000000, 0.000000000000000000 ) ) ;
#7327 = CARTESIAN_POINT ( 'NONE',  ( 0.000000000000000000, 0.000000000000000000, -154.5685424949238040 ) ) ;
#7328 = LINE ( 'NONE', #8080, #1816 ) ;
#7329 = DIRECTION ( 'NONE',  ( 1.000000000000000000, 0.000000000000000000, 0.000000000000000000 ) ) ;
#7330 = DIRECTION ( 'NONE',  ( 1.734723475976806848E-16, -1.000000000000000000, -0.000000000000000000 ) ) ;
#7331 = EDGE_CURVE ( 'NONE', #3529, #5790, #3082, .T. ) ;
#7332 = ORIENTED_EDGE ( 'NONE', *, *, #8521, .F. ) ;
#7333 = EDGE_CURVE ( 'NONE', #5730, #8171, #6298, .T. ) ;
#7334 = FILL_AREA_STYLE ('',( #4672 ) ) ;
#7335 = VERTEX_POINT ( 'NONE', #2521 ) ;
#7336 = AXIS2_PLACEMENT_3D ( 'NONE', #3154, #5797, #7811 ) ;
#7337 = ORIENTED_EDGE ( 'NONE', *, *, #5602, .T. ) ;
#7338 = FACE_OUTER_BOUND ( 'NONE', #1237, .T. ) ;
#7339 = LINE ( 'NONE', #4032, #7836 ) ;
#7340 = ORIENTED_EDGE ( 'NONE', *, *, #7636, .F. ) ;
#7341 = CARTESIAN_POINT ( 'NONE',  ( 20.00000000000000000, 175.0000000000000284, 5.000000000000000000 ) ) ;
#7342 = EDGE_LOOP ( 'NONE', ( #675, #1054, #1621, #3718 ) ) ;
#7343 = CARTESIAN_POINT ( 'NONE',  ( -4.999999999999998224, 140.0000000000000000, 15.00000000000000355 ) ) ;
#7344 = FACE_OUTER_BOUND ( 'NONE', #715, .T. ) ;
#7345 = APPLICATION_PROTOCOL_DEFINITION ( 'draft international standard', 'automotive_design', 1998, #351 ) ;
#7346 = EDGE_CURVE ( 'NONE', #7465, #2732, #8406, .T. ) ;
#7347 = PLANE ( 'NONE',  #150 ) ;
#7348 = VERTEX_POINT ( 'NONE', #8357 ) ;
#7349 = VERTEX_POINT ( 'NONE', #4992 ) ;
#7350 = CARTESIAN_POINT ( 'NONE',  ( -5.000000000000000000, -5.000000000000000000, 140.0000000000000000 ) ) ;
#7351 = FACE_OUTER_BOUND ( 'NONE', #169, .T. ) ;
#7352 = LINE ( 'NONE', #5255, #4270 ) ;
#7353 = VECTOR ( 'NONE', #2154, 1000.000000000000000 ) ;
#7354 = FACE_OUTER_BOUND ( 'NONE', #2267, .T. ) ;
#7355 = VERTEX_POINT ( 'NONE', #8446 ) ;
#7356 = VERTEX_POINT ( 'NONE', #1784 ) ;
#7357 = DIRECTION ( 'NONE',  ( 0.000000000000000000, -1.000000000000000000, 0.000000000000000000 ) ) ;
#7358 = AXIS2_PLACEMENT_3D ( 'NONE', #6971, #5576, #5537 ) ;
#7359 = CARTESIAN_POINT ( 'NONE',  ( 2.500000000000000000, 2.357898499370433054, -1.951563910473907981E-15 ) ) ;
#7360 = EDGE_CURVE ( 'NONE', #1782, #5393, #6008, .T. ) ;
#7361 = DIRECTION ( 'NONE',  ( -0.000000000000000000, 1.000000000000000000, -0.000000000000000000 ) ) ;
#7362 = ORIENTED_EDGE ( 'NONE', *, *, #8287, .F. ) ;
#7363 = LINE ( 'NONE', #6749, #7785 ) ;
#7364 = AXIS2_PLACEMENT_3D ( 'NONE', #313, #4848, #933 ) ;
#7365 = ADVANCED_FACE ( 'NONE', ( #7786 ), #2997, .F. ) ;
#7366 = CARTESIAN_POINT ( 'NONE',  ( 5.000000000000000000, -5.000000000000000000, 148.0000000000000284 ) ) ;
#7367 = EDGE_CURVE ( 'NONE', #2805, #8587, #1826, .T. ) ;
#7368 = LINE ( 'NONE', #2760, #7116 ) ;
#7369 = AXIS2_PLACEMENT_3D ( 'NONE', #8454, #294, #1830 ) ;
#7370 = CYLINDRICAL_SURFACE ( 'NONE', #4722, 2.649999999999985700 ) ;
#7371 = DIRECTION ( 'NONE',  ( 0.000000000000000000, 0.000000000000000000, 1.000000000000000000 ) ) ;
#7372 = DIRECTION ( 'NONE',  ( -1.000000000000000000, 0.000000000000000000, -0.000000000000000000 ) ) ;
#7373 = ORIENTED_EDGE ( 'NONE', *, *, #8388, .T. ) ;
#7374 = EDGE_LOOP ( 'NONE', ( #5814, #7869, #7803, #5703 ) ) ;
#7375 = UNCERTAINTY_MEASURE_WITH_UNIT (LENGTH_MEASURE( 1.000000000000000082E-05 ), #5199, 'distance_accuracy_value', 'NONE');
#7376 = ORIENTED_EDGE ( 'NONE', *, *, #3675, .T. ) ;
#7377 = LINE ( 'NONE', #2854, #892 ) ;
#7378 = CARTESIAN_POINT ( 'NONE',  ( 0.000000000000000000, 0.000000000000000000, 120.0000000000000142 ) ) ;
#7379 = ADVANCED_FACE ( 'NONE', ( #3171, #7864 ), #5846, .T. ) ;
#7380 = ORIENTED_EDGE ( 'NONE', *, *, #745, .T. ) ;
#7381 = DIRECTION ( 'NONE',  ( -1.000000000000000000, 0.000000000000000000, -0.000000000000000000 ) ) ;
#7382 = ORIENTED_EDGE ( 'NONE', *, *, #6233, .F. ) ;
#7383 = FACE_OUTER_BOUND ( 'NONE', #3256, .T. ) ;
#7384 = DIRECTION ( 'NONE',  ( -1.000000000000000000, 1.734723475976807587E-16, 0.000000000000000000 ) ) ;
#7385 = SHAPE_DEFINITION_REPRESENTATION ( #6766, #4754 ) ;
#7386 = ORIENTED_EDGE ( 'NONE', *, *, #5250, .F. ) ;
#7387 = ORIENTED_EDGE ( 'NONE', *, *, #5078, .F. ) ;
#7388 =( GEOMETRIC_REPRESENTATION_CONTEXT ( 3 ) GLOBAL_UNCERTAINTY_ASSIGNED_CONTEXT ( ( #5066 ) ) GLOBAL_UNIT_ASSIGNED_CONTEXT ( ( #5349, #7884, #6039 ) ) REPRESENTATION_CONTEXT ( 'NONE', 'WORKASPACE' ) );
#7389 = CARTESIAN_POINT ( 'NONE',  ( -4.000000000000000000, 0.000000000000000000, 0.000000000000000000 ) ) ;
#7390 = DIRECTION ( 'NONE',  ( -0.000000000000000000, 1.000000000000000000, -0.000000000000000000 ) ) ;
#7391 = DIRECTION ( 'NONE',  ( 1.000000000000000000, 0.000000000000000000, 0.000000000000000000 ) ) ;
#7392 = CONTEXT_DEPENDENT_SHAPE_REPRESENTATION ( #3585, #5729 ) ;
#7393 = PRODUCT ( 'single rail^MAS-188', 'single rail^MAS-188', '', ( #3215 ) ) ;
#7394 = DIRECTION ( 'NONE',  ( 1.000000000000000000, 0.000000000000000000, 0.000000000000000000 ) ) ;
#7395 = ORIENTED_EDGE ( 'NONE', *, *, #8595, .T. ) ;
#7396 = LINE ( 'NONE', #6174, #6845 ) ;
#7397 = ORIENTED_EDGE ( 'NONE', *, *, #6529, .T. ) ;
#7398 = ORIENTED_EDGE ( 'NONE', *, *, #442, .F. ) ;
#7399 = AXIS2_PLACEMENT_3D ( 'NONE', #2798, #1496, #4106 ) ;
#7400 = CARTESIAN_POINT ( 'NONE',  ( -2.687328764639638656, 3.067272167851286202, -0.05923475698270370959 ) ) ;
#7401 = AXIS2_PLACEMENT_3D ( 'NONE', #2285, #7540, #8246 ) ;
#7402 = CIRCLE ( 'NONE', #1719, 20.00000000000000000 ) ;
#7403 = DIRECTION ( 'NONE',  ( 0.000000000000000000, 0.5000000000000012212, 0.8660254037844380415 ) ) ;
#7404 = LINE ( 'NONE', #5914, #1928 ) ;
#7405 = ORIENTED_EDGE ( 'NONE', *, *, #6007, .T. ) ;
#7406 = FACE_OUTER_BOUND ( 'NONE', #8374, .T. ) ;
#7407 = EDGE_CURVE ( 'NONE', #1501, #3441, #3252, .T. ) ;
#7408 = VECTOR ( 'NONE', #8367, 1000.000000000000000 ) ;
#7409 = DIRECTION ( 'NONE',  ( 1.000000000000000000, 0.000000000000000000, 0.000000000000000000 ) ) ;
#7410 = VECTOR ( 'NONE', #5203, 1000.000000000000000 ) ;
#7411 = COLOUR_RGB ( '',0.8941176470588234615, 0.8941176470588234615, 0.8941176470588234615 ) ;
#7412 = CARTESIAN_POINT ( 'NONE',  ( 0.000000000000000000, 0.000000000000000000, 140.0000000000000000 ) ) ;
#7413 = ADVANCED_FACE ( 'NONE', ( #1208 ), #2685, .F. ) ;
#7414 = CARTESIAN_POINT ( 'NONE',  ( 386.6666666666666288, -20.00000000000000000, 165.1500000000000625 ) ) ;
#7415 = EDGE_CURVE ( 'NONE', #819, #1874, #7908, .T. ) ;
#7416 = CARTESIAN_POINT ( 'NONE',  ( 0.000000000000000000, 0.000000000000000000, 148.0000000000000284 ) ) ;
#7417 = CIRCLE ( 'NONE', #7147, 20.00000000000000000 ) ;
#7418 = ORIENTED_EDGE ( 'NONE', *, *, #3639, .F. ) ;
#7419 = ORIENTED_EDGE ( 'NONE', *, *, #7800, .T. ) ;
#7420 = VERTEX_POINT ( 'NONE', #4678 ) ;
#7421 = CARTESIAN_POINT ( 'NONE',  ( -5.000000000000000000, -5.000000000000000000, 34.00000000000000711 ) ) ;
#7422 = CARTESIAN_POINT ( 'NONE',  ( -31.74999999999995737, 0.000000000000000000, 4.250000000000000000 ) ) ;
#7423 = CIRCLE ( 'NONE', #7007, 20.00000000000000000 ) ;
#7424 = SHAPE_REPRESENTATION ( 'roller axis assy_r3', ( #594 ), #6685 ) ;
#7425 = VERTEX_POINT ( 'NONE', #3903 ) ;
#7426 = CARTESIAN_POINT ( 'NONE',  ( -30.00000000000002842, -25.00000000000000000, 200.0000000000000000 ) ) ;
#7427 = ORIENTED_EDGE ( 'NONE', *, *, #4391, .F. ) ;
#7428 = CARTESIAN_POINT ( 'NONE',  ( -5.000000000000001776, 5.000000000000001776, 148.0000000000000284 ) ) ;
#7429 = DIRECTION ( 'NONE',  ( -0.000000000000000000, 0.000000000000000000, -1.000000000000000000 ) ) ;
#7430 = APPLICATION_PROTOCOL_DEFINITION ( 'draft international standard', 'automotive_design', 1998, #6415 ) ;
#7431 = LINE ( 'NONE', #4163, #7688 ) ;
#7432 = ORIENTED_EDGE ( 'NONE', *, *, #8469, .F. ) ;
#7433 = ORIENTED_EDGE ( 'NONE', *, *, #4360, .F. ) ;
#7434 = CARTESIAN_POINT ( 'NONE',  ( 5.000000000000000000, -5.000000000000000000, 42.00000000000000711 ) ) ;
#7435 = FACE_OUTER_BOUND ( 'NONE', #5695, .T. ) ;
#7436 = CARTESIAN_POINT ( 'NONE',  ( 2.500000000000000000, 2.357898499370433054, -1.951563910473907981E-15 ) ) ;
#7437 = CARTESIAN_POINT ( 'NONE',  ( 1.411581201560190495E-15, 4.862606272033091592, -3.745885042887436622 ) ) ;
#7438 = ORIENTED_EDGE ( 'NONE', *, *, #1375, .T. ) ;
#7439 = DIRECTION ( 'NONE',  ( -0.000000000000000000, -0.000000000000000000, -1.000000000000000000 ) ) ;
#7440 = EDGE_CURVE ( 'NONE', #1525, #147, #636, .T. ) ;
#7441 = PRESENTATION_STYLE_ASSIGNMENT (( #788 ) ) ;
#7442 = DIRECTION ( 'NONE',  ( 1.000000000000000000, 0.000000000000000000, 0.000000000000000000 ) ) ;
#7443 = EDGE_CURVE ( 'NONE', #5265, #58, #1950, .T. ) ;
#7444 = ORIENTED_EDGE ( 'NONE', *, *, #1401, .T. ) ;
#7445 = CARTESIAN_POINT ( 'NONE',  ( -0.6640947660597427138, 4.471078309994878985, -3.602146406945963442 ) ) ;
#7446 = DIRECTION ( 'NONE',  ( 0.000000000000000000, 0.000000000000000000, 1.000000000000000000 ) ) ;
#7447 = CARTESIAN_POINT ( 'NONE',  ( 93.00000000000000000, 5.000000000000000000, 139.9990000000000236 ) ) ;
#7448 = ORIENTED_EDGE ( 'NONE', *, *, #5181, .F. ) ;
#7449 = FACE_OUTER_BOUND ( 'NONE', #3112, .T. ) ;
#7450 = LINE ( 'NONE', #3621, #4481 ) ;
#7451 = EDGE_CURVE ( 'NONE', #7275, #104, #7203, .T. ) ;
#7452 = VECTOR ( 'NONE', #3469, 1000.000000000000000 ) ;
#7453 = DIRECTION ( 'NONE',  ( -0.000000000000000000, 1.000000000000000000, -0.000000000000000000 ) ) ;
#7454 = DIRECTION ( 'NONE',  ( -1.734723475976806848E-16, 1.000000000000000000, 0.000000000000000000 ) ) ;
#7455 = VECTOR ( 'NONE', #1452, 1000.000000000000227 ) ;
#7456 = DIRECTION ( 'NONE',  ( -1.000000000000000000, 0.000000000000000000, -0.000000000000000000 ) ) ;
#7457 = CARTESIAN_POINT ( 'NONE',  ( -30.00000000000002842, -15.00000000000000000, 180.0000000000000284 ) ) ;
#7458 = AXIS2_PLACEMENT_3D ( 'NONE', #3663, #2968, #5486 ) ;
#7459 = VERTEX_POINT ( 'NONE', #1909 ) ;
#7460 = EDGE_LOOP ( 'NONE', ( #7398, #3484, #4598 ) ) ;
#7461 = ORIENTED_EDGE ( 'NONE', *, *, #6019, .T. ) ;
#7462 = DIRECTION ( 'NONE',  ( -1.000000000000000000, 0.000000000000000000, 0.000000000000000000 ) ) ;
#7463 = SURFACE_SIDE_STYLE ('',( #4723 ) ) ;
#7464 = PRODUCT ( 'roller axis assy_r6', 'roller axis assy_r6', '', ( #7631 ) ) ;
#7465 = VERTEX_POINT ( 'NONE', #1327 ) ;
#7466 = FACE_OUTER_BOUND ( 'NONE', #4283, .T. ) ;
#7467 = EDGE_CURVE ( 'NONE', #6024, #874, #3292, .T. ) ;
#7468 = ORIENTED_EDGE ( 'NONE', *, *, #6233, .T. ) ;
#7469 = CARTESIAN_POINT ( 'NONE',  ( 5.000000000000000000, 5.000000000000000000, -0.9999999999999940048 ) ) ;
#7470 = APPLICATION_CONTEXT ( 'automotive_design' ) ;
#7471 = DIRECTION ( 'NONE',  ( 0.000000000000000000, 1.000000000000000000, 0.000000000000000000 ) ) ;
#7472 = ADVANCED_FACE ( 'NONE', ( #1870 ), #3994, .F. ) ;
#7473 = APPLICATION_PROTOCOL_DEFINITION ( 'draft international standard', 'automotive_design', 1998, #7921 ) ;
#7474 = SURFACE_STYLE_FILL_AREA ( #4208 ) ;
#7475 = EDGE_LOOP ( 'NONE', ( #8084, #3449, #5902, #3599, #96 ) ) ;
#7476 = ORIENTED_EDGE ( 'NONE', *, *, #7756, .F. ) ;
#7477 = DIRECTION ( 'NONE',  ( -0.000000000000000000, 1.000000000000000000, -0.000000000000000000 ) ) ;
#7478 = EDGE_CURVE ( 'NONE', #5031, #2500, #6706, .T. ) ;
#7479 = CARTESIAN_POINT ( 'NONE',  ( 0.000000000000000000, 0.000000000000000000, -49.56854249492377562 ) ) ;
#7480 = DIRECTION ( 'NONE',  ( 0.000000000000000000, 0.000000000000000000, 1.000000000000000000 ) ) ;
#7481 = DIRECTION ( 'NONE',  ( -0.000000000000000000, -0.000000000000000000, 1.000000000000000000 ) ) ;
#7482 = ORIENTED_EDGE ( 'NONE', *, *, #1759, .T. ) ;
#7483 = CARTESIAN_POINT ( 'NONE',  ( -20.00000000000000000, 175.0000000000000284, 0.000000000000000000 ) ) ;
#7484 = CIRCLE ( 'NONE', #7634, 2.649999999999985700 ) ;
#7485 = DIRECTION ( 'NONE',  ( 0.000000000000000000, 0.000000000000000000, 1.000000000000000000 ) ) ;
#7486 = FACE_OUTER_BOUND ( 'NONE', #3341, .T. ) ;
#7487 = EDGE_LOOP ( 'NONE', ( #6191, #2123, #6748, #6519 ) ) ;
#7488 = CARTESIAN_POINT ( 'NONE',  ( 303.3333333333333144, -20.00000000000000000, 165.1500000000000625 ) ) ;
#7489 = PLANE ( 'NONE',  #6868 ) ;
#7490 = EDGE_CURVE ( 'NONE', #3102, #5372, #6545, .T. ) ;
#7491 = VECTOR ( 'NONE', #6056, 1000.000000000000000 ) ;
#7492 = DIRECTION ( 'NONE',  ( 1.000000000000000000, 0.000000000000000000, 0.000000000000000000 ) ) ;
#7493 = FACE_OUTER_BOUND ( 'NONE', #6942, .T. ) ;
#7494 = ORIENTED_EDGE ( 'NONE', *, *, #899, .T. ) ;
#7495 = CARTESIAN_POINT ( 'NONE',  ( 0.000000000000000000, 0.000000000000000000, 0.000000000000000000 ) ) ;
#7496 =( NAMED_UNIT ( * ) PLANE_ANGLE_UNIT ( ) SI_UNIT ( $, .RADIAN. ) );
#7497 = AXIS2_PLACEMENT_3D ( 'NONE', #7495, #927, #307 ) ;
#7498 = DIRECTION ( 'NONE',  ( -0.000000000000000000, -0.000000000000000000, 1.000000000000000000 ) ) ;
#7499 = DIRECTION ( 'NONE',  ( 0.000000000000000000, 0.000000000000000000, -1.000000000000000000 ) ) ;
#7500 = VECTOR ( 'NONE', #6188, 1000.000000000000000 ) ;
#7501 = CARTESIAN_POINT ( 'NONE',  ( 0.000000000000000000, 0.000000000000000000, 42.00000000000000711 ) ) ;
#7502 = PRODUCT_DEFINITION ( 'UNKNOWN', '', #5578, #1246 ) ;
#7503 = CARTESIAN_POINT ( 'NONE',  ( -0.6810597143197697489, -4.461075778259609770, -3.598441714920717516 ) ) ;
#7504 = CARTESIAN_POINT ( 'NONE',  ( 0.000000000000000000, 0.000000000000000000, -7.999999999999992895 ) ) ;
#7505 = EDGE_LOOP ( 'NONE', ( #5170, #4982, #420, #7448 ) ) ;
#7506 = VERTEX_POINT ( 'NONE', #1286 ) ;
#7507 = ORIENTED_EDGE ( 'NONE', *, *, #8090, .F. ) ;
#7508 = DIRECTION ( 'NONE',  ( 1.000000000000000000, 0.000000000000000000, 0.000000000000000000 ) ) ;
#7509 = VECTOR ( 'NONE', #6452, 1000.000000000000000 ) ;
#7510 = CARTESIAN_POINT ( 'NONE',  ( 5.000000000000000000, -5.000000000000000000, -63.99999999999997158 ) ) ;
#7511 = EDGE_LOOP ( 'NONE', ( #4435, #1729, #3922, #2529 ) ) ;
#7512 = CARTESIAN_POINT ( 'NONE',  ( -5.000000000000001776, 5.000000000000001776, 7.000000000000006217 ) ) ;
#7513 = EDGE_LOOP ( 'NONE', ( #4219, #5579, #4054, #8331 ) ) ;
#7514 = CARTESIAN_POINT ( 'NONE',  ( 1.393927851585479161, -4.043713361053543842, -3.526374918436840922 ) ) ;
#7515 = CARTESIAN_POINT ( 'NONE',  ( 5.000000000000000000, -5.000000000000000000, 148.0000000000000284 ) ) ;
#7516 = SHAPE_DEFINITION_REPRESENTATION ( #3225, #1479 ) ;
#7517 = PRESENTATION_STYLE_ASSIGNMENT (( #4863 ) ) ;
#7518 = ORIENTED_EDGE ( 'NONE', *, *, #8070, .T. ) ;
#7519 = EDGE_CURVE ( 'NONE', #3408, #4775, #3141, .T. ) ;
#7520 = VERTEX_POINT ( 'NONE', #5933 ) ;
#7521 = DIRECTION ( 'NONE',  ( 0.000000000000000000, 0.000000000000000000, 1.000000000000000000 ) ) ;
#7522 = CARTESIAN_POINT ( 'NONE',  ( 5.000000000000000000, -5.000000000000000000, 148.0000000000000284 ) ) ;
#7523 = EDGE_CURVE ( 'NONE', #6097, #3102, #7339, .T. ) ;
#7524 = EDGE_CURVE ( 'NONE', #6071, #479, #3338, .T. ) ;
#7525 = LINE ( 'NONE', #5124, #7305 ) ;
#7526 = CARTESIAN_POINT ( 'NONE',  ( 1.243802165048773611, -3.900692638707475624, -3.223146290109810241 ) ) ;
#7527 = EDGE_LOOP ( 'NONE', ( #7883, #7666, #7332, #4766 ) ) ;
#7528 = EDGE_CURVE ( 'NONE', #3247, #7506, #680, .T. ) ;
#7529 = CARTESIAN_POINT ( 'NONE',  ( -5.000000000000000000, -5.000000000000000000, 7.000000000000006217 ) ) ;
#7530 = ORIENTED_EDGE ( 'NONE', *, *, #4807, .F. ) ;
#7531 = ORIENTED_EDGE ( 'NONE', *, *, #7818, .T. ) ;
#7532 = CARTESIAN_POINT ( 'NONE',  ( -3.522875095019672109, 2.820352903225427532, -3.598441714920591394 ) ) ;
#7533 = CARTESIAN_POINT ( 'NONE',  ( -20.00000000000000000, 2.449293598294706513E-15, -77.99999999999997158 ) ) ;
#7534 = AXIS2_PLACEMENT_3D ( 'NONE', #8410, #4393, #2448 ) ;
#7535 = CARTESIAN_POINT ( 'NONE',  ( 0.000000000000000000, 0.000000000000000000, 140.0000000000000000 ) ) ;
#7536 = DIRECTION ( 'NONE',  ( -0.000000000000000000, -0.000000000000000000, 1.000000000000000000 ) ) ;
#7537 = ORIENTED_EDGE ( 'NONE', *, *, #6669, .F. ) ;
#7538 = FACE_BOUND ( 'NONE', #4349, .T. ) ;
#7539 = ORIENTED_EDGE ( 'NONE', *, *, #7795, .T. ) ;
#7540 = DIRECTION ( 'NONE',  ( 0.000000000000000000, 0.000000000000000000, -1.000000000000000000 ) ) ;
#7541 = AXIS2_PLACEMENT_3D ( 'NONE', #4365, #5096, #1802 ) ;
#7542 = CARTESIAN_POINT ( 'NONE',  ( 5.000000000000000000, -5.000000000000000000, -36.00000000000000000 ) ) ;
#7543 = VECTOR ( 'NONE', #5433, 1000.000000000000000 ) ;
#7544 = VECTOR ( 'NONE', #5514, 1000.000000000000000 ) ;
#7545 = CARTESIAN_POINT ( 'NONE',  ( -5.000000000000000000, -5.000000000000000000, -143.0000000000000284 ) ) ;
#7546 = AXIS2_PLACEMENT_3D ( 'NONE', #920, #255, #5564 ) ;
#7547 = CARTESIAN_POINT ( 'NONE',  ( 5.000000000000000000, 5.000000000000000000, -71.99999999999998579 ) ) ;
#7548 = DIRECTION ( 'NONE',  ( -0.000000000000000000, 1.000000000000000000, -0.000000000000000000 ) ) ;
#7549 = VERTEX_POINT ( 'NONE', #56 ) ;
#7550 = VECTOR ( 'NONE', #7294, 1000.000000000000000 ) ;
#7551 =( GEOMETRIC_REPRESENTATION_CONTEXT ( 3 ) GLOBAL_UNCERTAINTY_ASSIGNED_CONTEXT ( ( #1369 ) ) GLOBAL_UNIT_ASSIGNED_CONTEXT ( ( #4293, #5028, #6379 ) ) REPRESENTATION_CONTEXT ( 'NONE', 'WORKASPACE' ) );
#7552 = VERTEX_POINT ( 'NONE', #7827 ) ;
#7553 = EDGE_CURVE ( 'NONE', #478, #3529, #897, .T. ) ;
#7554 = EDGE_CURVE ( 'NONE', #5384, #133, #4770, .T. ) ;
#7555 = VERTEX_POINT ( 'NONE', #1547 ) ;
#7556 = LINE ( 'NONE', #5584, #4089 ) ;
#7557 = EDGE_CURVE ( 'NONE', #8142, #4780, #317, .T. ) ;
#7558 =( LENGTH_UNIT ( ) NAMED_UNIT ( * ) SI_UNIT ( .MILLI., .METRE. ) );
#7559 = AXIS2_PLACEMENT_3D ( 'NONE', #4457, #2343, #1112 ) ;
#7560 = STYLED_ITEM ( 'NONE', ( #218 ), #759 ) ;
#7561 = VERTEX_POINT ( 'NONE', #8133 ) ;
#7562 = CARTESIAN_POINT ( 'NONE',  ( 264.0000000000000000, -25.00000000000000000, -48.78142504031547588 ) ) ;
#7563 = ORIENTED_EDGE ( 'NONE', *, *, #4461, .F. ) ;
#7564 = DIRECTION ( 'NONE',  ( 0.000000000000000000, -0.000000000000000000, -1.000000000000000000 ) ) ;
#7565 = CONTEXT_DEPENDENT_SHAPE_REPRESENTATION ( #6299, #3507 ) ;
#7566 = DIRECTION ( 'NONE',  ( -1.000000000000000000, 1.734723475976807587E-16, 0.000000000000000000 ) ) ;
#7567 = VERTEX_POINT ( 'NONE', #7510 ) ;
#7568 = VERTEX_POINT ( 'NONE', #4198 ) ;
#7569 = AXIS2_PLACEMENT_3D ( 'NONE', #8553, #5192, #3812 ) ;
#7570 = DIRECTION ( 'NONE',  ( 1.000000000000000000, 0.000000000000000000, 0.000000000000000000 ) ) ;
#7571 = EDGE_CURVE ( 'NONE', #6564, #5265, #8218, .T. ) ;
#7572 = CARTESIAN_POINT ( 'NONE',  ( 20.00000000000000000, 0.000000000000000000, -14.56854249492377207 ) ) ;
#7573 = MANIFOLD_SOLID_BREP ( 'EndChamfer', #5224 ) ;
#7574 = VECTOR ( 'NONE', #2918, 1000.000000000000000 ) ;
#7575 = DIRECTION ( 'NONE',  ( -0.000000000000000000, 1.000000000000000000, -0.000000000000000000 ) ) ;
#7576 = DIRECTION ( 'NONE',  ( -0.5000000000000019984, -0.8660254037844375974, 0.000000000000000000 ) ) ;
#7577 = ORIENTED_EDGE ( 'NONE', *, *, #4278, .F. ) ;
#7578 = PLANE ( 'NONE',  #4621 ) ;
#7579 = VERTEX_POINT ( 'NONE', #2111 ) ;
#7580 = ORIENTED_EDGE ( 'NONE', *, *, #3420, .F. ) ;
#7581 = CARTESIAN_POINT ( 'NONE',  ( -4.141042297810615835, 2.227970268150415656, -3.687027686973619822 ) ) ;
#7582 = DIRECTION ( 'NONE',  ( 1.000000000000000000, 0.000000000000000000, 0.000000000000000000 ) ) ;
#7583 = ADVANCED_FACE ( 'NONE', ( #4075 ), #6104, .F. ) ;
#7584 = LINE ( 'NONE', #6224, #7045 ) ;
#7585 = PLANE ( 'NONE',  #3316 ) ;
#7586 = EDGE_LOOP ( 'NONE', ( #8270, #5410, #558, #6608 ) ) ;
#7587 = CARTESIAN_POINT ( 'NONE',  ( -3.511755186886750479, 2.826662030176366081, -3.597382984111578086 ) ) ;
#7588 =( NAMED_UNIT ( * ) SI_UNIT ( $, .STERADIAN. ) SOLID_ANGLE_UNIT ( ) );
#7589 = MANIFOLD_SOLID_BREP ( 'Boss-Extrude4', #7306 ) ;
#7590 = FACE_OUTER_BOUND ( 'NONE', #74, .T. ) ;
#7591 = ADVANCED_FACE ( 'NONE', ( #2727 ), #2160, .F. ) ;
#7592 = ADVANCED_FACE ( 'NONE', ( #770 ), #7648, .F. ) ;
#7593 = CARTESIAN_POINT ( 'NONE',  ( 444.9999999999999432, -4.999999999999998224, 140.0000000000000000 ) ) ;
#7594 = VECTOR ( 'NONE', #1182, 1000.000000000000000 ) ;
#7595 = CARTESIAN_POINT ( 'NONE',  ( 136.6666666666666288, -14.99999999999999822, 159.8500000000001080 ) ) ;
#7596 = CARTESIAN_POINT ( 'NONE',  ( -3.540020015735593439, -2.810662092924100630, -3.602146406945814672 ) ) ;
#7597 = ORIENTED_EDGE ( 'NONE', *, *, #3865, .F. ) ;
#7598 = CIRCLE ( 'NONE', #4257, 0.5155456020628804703 ) ;
#7599 = ORIENTED_EDGE ( 'NONE', *, *, #7467, .F. ) ;
#7600 = CLOSED_SHELL ( 'NONE', ( #3782, #8440, #5917, #6461, #223, #8124, #3273, #6307, #484, #5099, #6993, #824, #329, #708, #4763, #1473, #3753, #3879, #4442, #3191 ) ) ;
#7601 = ORIENTED_EDGE ( 'NONE', *, *, #6611, .F. ) ;
#7602 = LINE ( 'NONE', #4243, #2436 ) ;
#7603 = CARTESIAN_POINT ( 'NONE',  ( 136.6666666666666288, -20.00000000000000000, 165.1500000000000625 ) ) ;
#7604 = VECTOR ( 'NONE', #6627, 1000.000000000000000 ) ;
#7605 = EDGE_CURVE ( 'NONE', #3816, #2989, #321, .T. ) ;
#7606 = AXIS2_PLACEMENT_3D ( 'NONE', #2713, #796, #6879 ) ;
#7607 = ORIENTED_EDGE ( 'NONE', *, *, #1844, .F. ) ;
#7608 = CARTESIAN_POINT ( 'NONE',  ( 10.00000000000000000, 0.000000000000000000, 120.0000000000000142 ) ) ;
#7609 = VERTEX_POINT ( 'NONE', #2987 ) ;
#7610 = CARTESIAN_POINT ( 'NONE',  ( 0.000000000000000000, 0.000000000000000000, 62.00000000000001421 ) ) ;
#7611 = CONTEXT_DEPENDENT_SHAPE_REPRESENTATION ( #4364, #7183 ) ;
#7612 =( NAMED_UNIT ( * ) SI_UNIT ( $, .STERADIAN. ) SOLID_ANGLE_UNIT ( ) );
#7613 = ORIENTED_EDGE ( 'NONE', *, *, #249, .T. ) ;
#7614 = VERTEX_POINT ( 'NONE', #410 ) ;
#7615 = DIRECTION ( 'NONE',  ( 0.000000000000000000, 0.000000000000000000, 1.000000000000000000 ) ) ;
#7616 = CYLINDRICAL_SURFACE ( 'NONE', #1860, 10.00000000000000000 ) ;
#7617 = DIRECTION ( 'NONE',  ( -1.000000000000000000, 0.000000000000000000, 0.000000000000000000 ) ) ;
#7618 = LINE ( 'NONE', #4997, #6649 ) ;
#7619 = ORIENTED_EDGE ( 'NONE', *, *, #8016, .F. ) ;
#7620 = DIRECTION ( 'NONE',  ( 0.000000000000000000, 0.000000000000000000, -1.000000000000000000 ) ) ;
#7621 = EDGE_LOOP ( 'NONE', ( #7023, #2852, #3679, #2340 ) ) ;
#7622 = ADVANCED_BREP_SHAPE_REPRESENTATION ( '', ( #4757, #594 ), #1167 ) ;
#7623 = ORIENTED_EDGE ( 'NONE', *, *, #6716, .F. ) ;
#7624 = LINE ( 'NONE', #1002, #7270 ) ;
#7625 = VECTOR ( 'NONE', #7361, 1000.000000000000000 ) ;
#7626 = LINE ( 'NONE', #3490, #6578 ) ;
#7627 = PLANE ( 'NONE',  #5230 ) ;
#7628 = FACE_OUTER_BOUND ( 'NONE', #3335, .T. ) ;
#7629 = ORIENTED_EDGE ( 'NONE', *, *, #2103, .F. ) ;
#7630 = PLANE ( 'NONE',  #4023 ) ;
#7631 = PRODUCT_CONTEXT ( 'NONE', #6744, 'mechanical' ) ;
#7632 = ORIENTED_EDGE ( 'NONE', *, *, #3565, .F. ) ;
#7633 = DIRECTION ( 'NONE',  ( -1.000000000000000000, 1.734723475976807587E-16, 0.000000000000000000 ) ) ;
#7634 = AXIS2_PLACEMENT_3D ( 'NONE', #3310, #3921, #5949 ) ;
#7635 = DIRECTION ( 'NONE',  ( 0.000000000000000000, 0.000000000000000000, 1.000000000000000000 ) ) ;
#7636 = EDGE_CURVE ( 'NONE', #848, #6900, #6414, .T. ) ;
#7637 = EDGE_CURVE ( 'NONE', #2573, #5816, #4087, .T. ) ;
#7638 = CARTESIAN_POINT ( 'NONE',  ( 357.0000000000000000, -4.999999999999998224, 140.0000000000000000 ) ) ;
#7639 = EDGE_CURVE ( 'NONE', #5790, #3653, #4942, .T. ) ;
#7640 = DIRECTION ( 'NONE',  ( -0.000000000000000000, 0.000000000000000000, 1.000000000000000000 ) ) ;
#7641 = CARTESIAN_POINT ( 'NONE',  ( -4.000000000000000000, 0.8730739991738342143, -3.223134629628428893 ) ) ;
#7642 = VECTOR ( 'NONE', #2616, 1000.000000000000000 ) ;
#7643 = ORIENTED_EDGE ( 'NONE', *, *, #5262, .T. ) ;
#7644 = EDGE_CURVE ( 'NONE', #1691, #5766, #4915, .T. ) ;
#7645 = ORIENTED_EDGE ( 'NONE', *, *, #661, .T. ) ;
#7646 = VERTEX_POINT ( 'NONE', #8431 ) ;
#7647 = CARTESIAN_POINT ( 'NONE',  ( 0.000000000000000000, 0.000000000000000000, 140.0000000000000000 ) ) ;
#7648 = CYLINDRICAL_SURFACE ( 'NONE', #7559, 2.649999999999985700 ) ;
#7649 =( REPRESENTATION_RELATIONSHIP ('NONE','NONE', #3312, #1479 ) REPRESENTATION_RELATIONSHIP_WITH_TRANSFORMATION ( #5465 )SHAPE_REPRESENTATION_RELATIONSHIP( ) );
#7650 = CIRCLE ( 'NONE', #3891, 2.649999999999985700 ) ;
#7651 = VERTEX_POINT ( 'NONE', #2300 ) ;
#7652 = ORIENTED_EDGE ( 'NONE', *, *, #6128, .T. ) ;
#7653 = CARTESIAN_POINT ( 'NONE',  ( 0.000000000000000000, 0.000000000000000000, 0.000000000000000000 ) ) ;
#7654 = DIRECTION ( 'NONE',  ( -0.000000000000000000, 1.000000000000000000, -0.000000000000000000 ) ) ;
#7655 = EDGE_LOOP ( 'NONE', ( #5245, #1799 ) ) ;
#7656 = VECTOR ( 'NONE', #4546, 1000.000000000000000 ) ;
#7657 = ORIENTED_EDGE ( 'NONE', *, *, #2700, .F. ) ;
#7658 = EDGE_CURVE ( 'NONE', #997, #8049, #469, .T. ) ;
#7659 = CARTESIAN_POINT ( 'NONE',  ( -31.74999999999995737, 0.000000000000000000, 0.000000000000000000 ) ) ;
#7660 = DIRECTION ( 'NONE',  ( 0.000000000000000000, 0.000000000000000000, -1.000000000000000000 ) ) ;
#7661 = CARTESIAN_POINT ( 'NONE',  ( 4.204015924366189871, -1.626724848190933548, -3.610627190413393084 ) ) ;
#7662 = CARTESIAN_POINT ( 'NONE',  ( 5.000000000000000000, 140.0000000000000000, 25.00000000000000000 ) ) ;
#7663 = VERTEX_POINT ( 'NONE', #7070 ) ;
#7664 = CARTESIAN_POINT ( 'NONE',  ( 439.9999999999999432, -20.00000000000003553, 176.4685749596844744 ) ) ;
#7665 = CYLINDRICAL_SURFACE ( 'NONE', #4869, 2.649999999999985700 ) ;
#7666 = ORIENTED_EDGE ( 'NONE', *, *, #4810, .F. ) ;
#7667 = ORIENTED_EDGE ( 'NONE', *, *, #4122, .F. ) ;
#7668 = EDGE_CURVE ( 'NONE', #5265, #7722, #1682, .T. ) ;
#7669 = CARTESIAN_POINT ( 'NONE',  ( 264.0000000000000000, -25.00000000000000000, -51.43142504031546025 ) ) ;
#7670 = EDGE_CURVE ( 'NONE', #530, #3740, #276, .T. ) ;
#7671 = CARTESIAN_POINT ( 'NONE',  ( 0.000000000000000000, 0.000000000000000000, -43.99999999999997158 ) ) ;
#7672 = EDGE_CURVE ( 'NONE', #337, #4682, #6979, .T. ) ;
#7673 = PLANE ( 'NONE',  #4944 ) ;
#7674 = STYLED_ITEM ( 'NONE', ( #7441 ), #5415 ) ;
#7675 = CARTESIAN_POINT ( 'NONE',  ( -30.00000000000000000, 15.00000000000000000, 140.0000000000000000 ) ) ;
#7676 = ORIENTED_EDGE ( 'NONE', *, *, #4886, .T. ) ;
#7677 = CARTESIAN_POINT ( 'NONE',  ( 20.00000000000000000, 0.000000000000000000, -115.0000000000000000 ) ) ;
#7678 = SHAPE_DEFINITION_REPRESENTATION ( #153, #4706 ) ;
#7679 = ORIENTED_EDGE ( 'NONE', *, *, #6719, .T. ) ;
#7680 = CARTESIAN_POINT ( 'NONE',  ( 0.000000000000000000, 0.000000000000000000, 120.0000000000000142 ) ) ;
#7681 = ORIENTED_EDGE ( 'NONE', *, *, #7044, .F. ) ;
#7682 = FACE_OUTER_BOUND ( 'NONE', #2772, .T. ) ;
#7683 = DIRECTION ( 'NONE',  ( 0.000000000000000000, 0.000000000000000000, 1.000000000000000000 ) ) ;
#7684 = ADVANCED_FACE ( 'NONE', ( #7027, #1068 ), #1029, .T. ) ;
#7685 = CARTESIAN_POINT ( 'NONE',  ( 2.682243648011666703, 3.070208061305304881, -0.04852650426601266831 ) ) ;
#7686 = SHAPE_REPRESENTATION ( 'roller axis assy_r5', ( #594 ), #1408 ) ;
#7687 = ORIENTED_EDGE ( 'NONE', *, *, #6750, .T. ) ;
#7688 = VECTOR ( 'NONE', #729, 1000.000000000000000 ) ;
#7689 = ORIENTED_EDGE ( 'NONE', *, *, #6506, .T. ) ;
#7690 = AXIS2_PLACEMENT_3D ( 'NONE', #2335, #2976, #6320 ) ;
#7691 = FACE_OUTER_BOUND ( 'NONE', #436, .T. ) ;
#7692 = CARTESIAN_POINT ( 'NONE',  ( 5.000000000000000000, 5.000000000000000000, 140.0000000000000000 ) ) ;
#7693 = UNCERTAINTY_MEASURE_WITH_UNIT (LENGTH_MEASURE( 1.000000000000000082E-05 ), #2030, 'distance_accuracy_value', 'NONE');
#7694 = PRODUCT_DEFINITION_SHAPE ( 'NONE', 'NONE',  #8634 ) ;
#7695 = VECTOR ( 'NONE', #531, 1000.000000000000000 ) ;
#7696 = EDGE_CURVE ( 'NONE', #5804, #6568, #4288, .T. ) ;
#7697 = ORIENTED_EDGE ( 'NONE', *, *, #5262, .F. ) ;
#7698 = PRESENTATION_LAYER_ASSIGNMENT (  '', '', ( #5315 ) ) ;
#7699 = VERTEX_POINT ( 'NONE', #7603 ) ;
#7700 = AXIS2_PLACEMENT_3D ( 'NONE', #8274, #993, #4340 ) ;
#7701 = FACE_OUTER_BOUND ( 'NONE', #8075, .T. ) ;
#7702 = EDGE_LOOP ( 'NONE', ( #6717, #7681, #61, #6526 ) ) ;
#7703 = AXIS2_PLACEMENT_3D ( 'NONE', #522, #3833, #7136 ) ;
#7704 = VERTEX_POINT ( 'NONE', #8389 ) ;
#7705 = PLANE ( 'NONE',  #3522 ) ;
#7706 =( GEOMETRIC_REPRESENTATION_CONTEXT ( 3 ) GLOBAL_UNCERTAINTY_ASSIGNED_CONTEXT ( ( #4071 ) ) GLOBAL_UNIT_ASSIGNED_CONTEXT ( ( #2770, #137, #6765 ) ) REPRESENTATION_CONTEXT ( 'NONE', 'WORKASPACE' ) );
#7707 = DIRECTION ( 'NONE',  ( -0.000000000000000000, -0.000000000000000000, 1.000000000000000000 ) ) ;
#7708 = CARTESIAN_POINT ( 'NONE',  ( 10.00000000000000000, 0.000000000000000000, 62.00000000000001421 ) ) ;
#7709 = CARTESIAN_POINT ( 'NONE',  ( -4.000000000000000000, -2.309401076758512694, -3.433295621305382461 ) ) ;
#7710 = ORIENTED_EDGE ( 'NONE', *, *, #7280, .F. ) ;
#7711 = AXIS2_PLACEMENT_3D ( 'NONE', #5108, #4500, #2552 ) ;
#7712 = DIRECTION ( 'NONE',  ( 2.081668171172168513E-17, 1.000000000000000222, 0.000000000000000000 ) ) ;
#7713 = DIRECTION ( 'NONE',  ( -0.000000000000000000, -0.000000000000000000, 1.000000000000000000 ) ) ;
#7714 = ORIENTED_EDGE ( 'NONE', *, *, #7644, .T. ) ;
#7715 = ORIENTED_EDGE ( 'NONE', *, *, #3689, .F. ) ;
#7716 = DIRECTION ( 'NONE',  ( -0.000000000000000000, 1.000000000000000000, -0.000000000000000000 ) ) ;
#7717 = DIRECTION ( 'NONE',  ( 1.000000000000000000, -1.734723475976806848E-16, 0.000000000000000000 ) ) ;
#7718 = AXIS2_PLACEMENT_3D ( 'NONE', #4601, #8536, #3965 ) ;
#7719 = CARTESIAN_POINT ( 'NONE',  ( 4.000000000000000000, -2.309401076758516691, -0.4999999999999995559 ) ) ;
#7720 = EDGE_CURVE ( 'NONE', #1874, #5745, #2938, .T. ) ;
#7721 = FACE_OUTER_BOUND ( 'NONE', #295, .T. ) ;
#7722 = VERTEX_POINT ( 'NONE', #7692 ) ;
#7723 = EDGE_CURVE ( 'NONE', #7722, #2735, #1638, .T. ) ;
#7724 = ORIENTED_EDGE ( 'NONE', *, *, #4261, .T. ) ;
#7725 = CARTESIAN_POINT ( 'NONE',  ( 4.175002511812151873, 2.208363329454889445, -3.469254087858244073 ) ) ;
#7726 = CARTESIAN_POINT ( 'NONE',  ( -5.000000000000001776, 5.000000000000001776, 140.0000000000000000 ) ) ;
#7727 = DIRECTION ( 'NONE',  ( 0.000000000000000000, 0.000000000000000000, -1.000000000000000000 ) ) ;
#7728 = LINE ( 'NONE', #2465, #5272 ) ;
#7729 = DIRECTION ( 'NONE',  ( -1.000000000000000000, -0.000000000000000000, -0.000000000000000000 ) ) ;
#7730 = LINE ( 'NONE', #8383, #935 ) ;
#7732 = ORIENTED_EDGE ( 'NONE', *, *, #914, .F. ) ;
#7731 = EDGE_CURVE ( 'NONE', #6999, #7972, #1869, .T. ) ;
#7733 = DIRECTION ( 'NONE',  ( -0.000000000000000000, 1.000000000000000000, -0.000000000000000000 ) ) ;
#7734 = AXIS2_PLACEMENT_3D ( 'NONE', #4695, #1390, #4046 ) ;
#7735 = DIRECTION ( 'NONE',  ( 1.000000000000000000, -1.734723475976806848E-16, 0.000000000000000000 ) ) ;
#7736 = LINE ( 'NONE', #1771, #2696 ) ;
#7737 = ORIENTED_EDGE ( 'NONE', *, *, #7897, .F. ) ;
#7738 = TOROIDAL_SURFACE ( 'NONE', #6338, 4.000000000000000000, 0.2500000000000000000 ) ;
#7739 = PLANE ( 'NONE',  #1757 ) ;
#7740 = ORIENTED_EDGE ( 'NONE', *, *, #14, .F. ) ;
#7741 = SURFACE_STYLE_USAGE ( .BOTH. , #8399 ) ;
#7742 = CARTESIAN_POINT ( 'NONE',  ( 470.0000000000000000, -20.00000000000000000, 200.0000000000000000 ) ) ;
#7743 = EDGE_LOOP ( 'NONE', ( #1047, #5611 ) ) ;
#7744 = EDGE_LOOP ( 'NONE', ( #5467, #3004, #8137, #2242 ) ) ;
#7745 = DIRECTION ( 'NONE',  ( -0.000000000000000000, -0.000000000000000000, 1.000000000000000000 ) ) ;
#7746 = CARTESIAN_POINT ( 'NONE',  ( -5.000000000000000000, -5.000000000000000000, 148.0000000000000284 ) ) ;
#7747 = MECHANICAL_DESIGN_GEOMETRIC_PRESENTATION_REPRESENTATION (  '', ( #8164 ), #1342 ) ;
#7748 = CIRCLE ( 'NONE', #5092, 2.649999999999985700 ) ;
#7749 = EDGE_CURVE ( 'NONE', #5488, #958, #8306, .T. ) ;
#7750 = DIRECTION ( 'NONE',  ( -1.734723475976806848E-16, 1.000000000000000000, 0.000000000000000000 ) ) ;
#7751 = VERTEX_POINT ( 'NONE', #5065 ) ;
#7752 = AXIS2_PLACEMENT_3D ( 'NONE', #572, #1268, #3197 ) ;
#7753 = DIRECTION ( 'NONE',  ( 6.123233995736766036E-17, -1.000000000000000000, 0.000000000000000000 ) ) ;
#7754 = CARTESIAN_POINT ( 'NONE',  ( 0.000000000000000000, 0.000000000000000000, -27.99999999999999645 ) ) ;
#7755 = EDGE_LOOP ( 'NONE', ( #7689, #828, #236, #7645 ) ) ;
#7756 = EDGE_CURVE ( 'NONE', #8365, #7335, #7736, .T. ) ;
#7757 = ORIENTED_EDGE ( 'NONE', *, *, #3348, .F. ) ;
#7758 = CARTESIAN_POINT ( 'NONE',  ( 176.0000000000000000, -20.00000000000000000, -86.63142504031547730 ) ) ;
#7759 = LINE ( 'NONE', #1881, #7848 ) ;
#7760 = FACE_OUTER_BOUND ( 'NONE', #2819, .T. ) ;
#7761 = CYLINDRICAL_SURFACE ( 'NONE', #4560, 20.00000000000000000 ) ;
#7762 = ORIENTED_EDGE ( 'NONE', *, *, #1263, .F. ) ;
#7763 = ORIENTED_EDGE ( 'NONE', *, *, #580, .F. ) ;
#7764 = APPLICATION_CONTEXT ( 'automotive_design' ) ;
#7765 = DIRECTION ( 'NONE',  ( 0.000000000000000000, 1.000000000000000000, -1.287488025362403787E-15 ) ) ;
#7766 = ADVANCED_FACE ( 'NONE', ( #2673 ), #1274, .F. ) ;
#7767 = DIRECTION ( 'NONE',  ( -0.000000000000000000, -0.000000000000000000, 1.000000000000000000 ) ) ;
#7768 = DIRECTION ( 'NONE',  ( 0.000000000000000000, 1.000000000000000000, 0.000000000000000000 ) ) ;
#7769 = PLANE ( 'NONE',  #1671 ) ;
#7770 = CARTESIAN_POINT ( 'NONE',  ( -4.000000000000000000, 2.471528634177585282, -3.686887442155186712 ) ) ;
#7771 = ORIENTED_EDGE ( 'NONE', *, *, #1602, .T. ) ;
#7772 = AXIS2_PLACEMENT_3D ( 'NONE', #5658, #695, #1221 ) ;
#7773 = DIRECTION ( 'NONE',  ( -1.000000000000000000, 0.000000000000000000, 0.000000000000000000 ) ) ;
#7774 = CARTESIAN_POINT ( 'NONE',  ( 5.000000000000000000, -5.000000000000000000, 148.0000000000000284 ) ) ;
#7775 = CARTESIAN_POINT ( 'NONE',  ( 434.9999999999999432, -4.999999999999998224, 139.9990000000000236 ) ) ;
#7776 = VECTOR ( 'NONE', #3047, 1000.000000000000000 ) ;
#7777 = ORIENTED_EDGE ( 'NONE', *, *, #8072, .F. ) ;
#7778 = CARTESIAN_POINT ( 'NONE',  ( 303.3333333333333144, -25.00000000000000000, 159.8500000000001080 ) ) ;
#7779 = ORIENTED_EDGE ( 'NONE', *, *, #5969, .T. ) ;
#7780 = FACE_OUTER_BOUND ( 'NONE', #3061, .T. ) ;
#7781 = CONTEXT_DEPENDENT_SHAPE_REPRESENTATION ( #8537, #2192 ) ;
#7782 = ORIENTED_EDGE ( 'NONE', *, *, #1213, .F. ) ;
#7783 = ORIENTED_EDGE ( 'NONE', *, *, #1261, .F. ) ;
#7784 = LINE ( 'NONE', #2310, #499 ) ;
#7785 = VECTOR ( 'NONE', #6659, 1000.000000000000000 ) ;
#7786 = FACE_OUTER_BOUND ( 'NONE', #5206, .T. ) ;
#7787 = CARTESIAN_POINT ( 'NONE',  ( 4.197393957002303999, 7.772902908466098641E-14, -3.503767560748929810 ) ) ;
#7788 = AXIS2_PLACEMENT_3D ( 'NONE', #1404, #3367, #2 ) ;
#7789 = ORIENTED_EDGE ( 'NONE', *, *, #5472, .F. ) ;
#7790 = EDGE_CURVE ( 'NONE', #4735, #3602, #5966, .T. ) ;
#7791 = DIRECTION ( 'NONE',  ( 6.123233995736766036E-17, -1.000000000000000000, 0.000000000000000000 ) ) ;
#7792 = LINE ( 'NONE', #427, #8217 ) ;
#7793 = ORIENTED_EDGE ( 'NONE', *, *, #849, .T. ) ;
#7794 = EDGE_LOOP ( 'NONE', ( #6209, #2814, #944, #4918 ) ) ;
#7795 = EDGE_CURVE ( 'NONE', #7646, #5070, #7941, .T. ) ;
#7796 = DIRECTION ( 'NONE',  ( -0.000000000000000000, 1.000000000000000000, -0.000000000000000000 ) ) ;
#7797 = DIRECTION ( 'NONE',  ( -1.000000000000000000, -0.000000000000000000, -0.000000000000000000 ) ) ;
#7798 = AXIS2_PLACEMENT_3D ( 'NONE', #7189, #6321, #1720 ) ;
#7799 = EDGE_CURVE ( 'NONE', #716, #5045, #2513, .T. ) ;
#7800 = EDGE_CURVE ( 'NONE', #5335, #1123, #3982, .T. ) ;
#7801 = DIRECTION ( 'NONE',  ( 1.000000000000000000, 0.000000000000000000, 0.000000000000000000 ) ) ;
#7802 = LINE ( 'NONE', #2367, #6368 ) ;
#7803 = ORIENTED_EDGE ( 'NONE', *, *, #2488, .F. ) ;
#7804 = PRESENTATION_STYLE_ASSIGNMENT (( #3101 ) ) ;
#7805 = ORIENTED_EDGE ( 'NONE', *, *, #253, .F. ) ;
#7806 = ORIENTED_EDGE ( 'NONE', *, *, #1762, .F. ) ;
#7807 = DIRECTION ( 'NONE',  ( 0.000000000000000000, 0.000000000000000000, -1.000000000000000000 ) ) ;
#7808 = DIRECTION ( 'NONE',  ( 0.000000000000000000, 0.000000000000000000, -1.000000000000000000 ) ) ;
#7809 = DIRECTION ( 'NONE',  ( 0.000000000000000000, 0.000000000000000000, 1.000000000000000000 ) ) ;
#7810 = CARTESIAN_POINT ( 'NONE',  ( 434.9999999999999432, -4.999999999999998224, 145.0000000000000284 ) ) ;
#7811 = DIRECTION ( 'NONE',  ( -0.000000000000000000, 0.000000000000000000, 1.000000000000000000 ) ) ;
#7812 = CARTESIAN_POINT ( 'NONE',  ( 5.000000000000000000, -5.000000000000000000, -71.99999999999998579 ) ) ;
#7813 = DIRECTION ( 'NONE',  ( 0.000000000000000000, 1.000000000000000000, 0.000000000000000000 ) ) ;
#7814 = PLANE ( 'NONE',  #4061 ) ;
#7815 = CIRCLE ( 'NONE', #7772, 10.00000000000000000 ) ;
#7816=STYLED_ITEM('',(#8678),#4686);
#7817 =( NAMED_UNIT ( * ) SI_UNIT ( $, .STERADIAN. ) SOLID_ANGLE_UNIT ( ) );
#7818 = EDGE_CURVE ( 'NONE', #3609, #596, #4159, .T. ) ;
#7819 = ORIENTED_EDGE ( 'NONE', *, *, #2149, .F. ) ;
#7820 = EDGE_CURVE ( 'NONE', #6891, #5259, #4202, .T. ) ;
#7821 = AXIS2_PLACEMENT_3D ( 'NONE', #1584, #3714, #311 ) ;
#7822 = CARTESIAN_POINT ( 'NONE',  ( 5.000000000000000000, -5.000000000000000000, -135.0000000000000000 ) ) ;
#7823 = EDGE_CURVE ( 'NONE', #1985, #4980, #6499, .T. ) ;
#7824 = ORIENTED_EDGE ( 'NONE', *, *, #3036, .T. ) ;
#7825 = CARTESIAN_POINT ( 'NONE',  ( -4.999999999999998224, 135.0000000000000000, 15.00000000000000355 ) ) ;
#7826 = VECTOR ( 'NONE', #705, 1000.000000000000000 ) ;
#7827 = CARTESIAN_POINT ( 'NONE',  ( 4.000000000000000000, 0.000000000000000000, 0.000000000000000000 ) ) ;
#7828 = DIRECTION ( 'NONE',  ( 1.000000000000000000, -1.734723475976806848E-16, 0.000000000000000000 ) ) ;
#7829 = ORIENTED_EDGE ( 'NONE', *, *, #1375, .F. ) ;
#7830 = AXIS2_PLACEMENT_3D ( 'NONE', #4005, #8011, #25 ) ;
#7831 = CARTESIAN_POINT ( 'NONE',  ( 0.000000000000000000, 0.000000000000000000, 140.0000000000000000 ) ) ;
#7832 = CARTESIAN_POINT ( 'NONE',  ( 88.00000000000000000, -9.999999999999994671, -121.8314250403154659 ) ) ;
#7833 = ADVANCED_FACE ( 'NONE', ( #1 ), #5923, .T. ) ;
#7834 = DIRECTION ( 'NONE',  ( -0.000000000000000000, 1.000000000000000000, -0.000000000000000000 ) ) ;
#7835 = ORIENTED_EDGE ( 'NONE', *, *, #4724, .F. ) ;
#7836 = VECTOR ( 'NONE', #2642, 1000.000000000000000 ) ;
#7837 = EDGE_LOOP ( 'NONE', ( #7432, #1679 ) ) ;
#7838 = PRESENTATION_LAYER_ASSIGNMENT (  '', '', ( #8534 ) ) ;
#7839 = DIRECTION ( 'NONE',  ( -1.734723475976806848E-16, 1.000000000000000000, 0.000000000000000000 ) ) ;
#7840 = LINE ( 'NONE', #2496, #8276 ) ;
#7841 = AXIS2_PLACEMENT_3D ( 'NONE', #7896, #3855, #4537 ) ;
#7842 = AXIS2_PLACEMENT_3D ( 'NONE', #1681, #4375, #3722 ) ;
#7843 = CARTESIAN_POINT ( 'NONE',  ( 0.000000000000000000, 157.5000000000000284, 0.000000000000000000 ) ) ;
#7844 = CARTESIAN_POINT ( 'NONE',  ( 136.6666666666666288, -15.00000000000000000, 162.5000000000000853 ) ) ;
#7845 = ORIENTED_EDGE ( 'NONE', *, *, #3139, .T. ) ;
#7846 = ORIENTED_EDGE ( 'NONE', *, *, #4461, .T. ) ;
#7847 = CARTESIAN_POINT ( 'NONE',  ( 3.540020015735602765, 2.810662092924382627, -3.602146406945867962 ) ) ;
#7848 = VECTOR ( 'NONE', #8327, 1000.000000000000000 ) ;
#7849 = LINE ( 'NONE', #3803, #3713 ) ;
#7850 = FACE_OUTER_BOUND ( 'NONE', #1295, .T. ) ;
#7851 = CARTESIAN_POINT ( 'NONE',  ( 0.000000000000000000, 0.000000000000000000, -63.99999999999997158 ) ) ;
#7852 = PRESENTATION_STYLE_ASSIGNMENT (( #1314 ) ) ;
#7853 = VECTOR ( 'NONE', #4427, 1000.000000000000000 ) ;
#7854 = ADVANCED_FACE ( 'NONE', ( #1198 ), #7814, .F. ) ;
#7855 = EDGE_CURVE ( 'NONE', #8118, #186, #1318, .T. ) ;
#7856 = CARTESIAN_POINT ( 'NONE',  ( 357.0000000000000000, 5.000000000000000000, 145.0000000000000284 ) ) ;
#7857 = DIRECTION ( 'NONE',  ( 1.000000000000000000, -1.734723475976806848E-16, 0.000000000000000000 ) ) ;
#7858 = CARTESIAN_POINT ( 'NONE',  ( 3.999999999999999112, 2.309401076758497595, -3.504271511726784194 ) ) ;
#7859 = CARTESIAN_POINT ( 'NONE',  ( 5.000000000000000000, 5.000000000000000000, 148.0000000000000284 ) ) ;
#7860 = ORIENTED_EDGE ( 'NONE', *, *, #3064, .F. ) ;
#7861 = LINE ( 'NONE', #1865, #8437 ) ;
#7862 = ORIENTED_EDGE ( 'NONE', *, *, #6750, .F. ) ;
#7863 = FACE_OUTER_BOUND ( 'NONE', #4155, .T. ) ;
#7864 = FACE_OUTER_BOUND ( 'NONE', #1604, .T. ) ;
#7865 = EDGE_CURVE ( 'NONE', #7552, #5858, #3334, .T. ) ;
#7866 = PRODUCT_DEFINITION_CONTEXT ( 'detailed design', #1081, 'design' ) ;
#7867 = VECTOR ( 'NONE', #825, 1000.000000000000000 ) ;
#7868 = DIRECTION ( 'NONE',  ( -0.000000000000000000, 1.000000000000000000, -0.000000000000000000 ) ) ;
#7869 = ORIENTED_EDGE ( 'NONE', *, *, #3966, .F. ) ;
#7870 = DIRECTION ( 'NONE',  ( 1.000000000000000000, 0.000000000000000000, 0.000000000000000000 ) ) ;
#7871 = DIRECTION ( 'NONE',  ( -0.06393308594707912407, -3.914772225553873302E-18, -0.9979541875864260669 ) ) ;
#7872 = DIRECTION ( 'NONE',  ( 1.000000000000000000, 0.000000000000000000, 0.000000000000000000 ) ) ;
#7873 = EDGE_LOOP ( 'NONE', ( #5416, #6776, #4460, #3988 ) ) ;
#7874 = EDGE_LOOP ( 'NONE', ( #6543, #2934, #8442, #8343 ) ) ;
#7875 = VECTOR ( 'NONE', #3685, 1000.000000000000000 ) ;
#7877 = VECTOR ( 'NONE', #281, 1000.000000000000000 ) ;
#7876 = DIRECTION ( 'NONE',  ( 0.000000000000000000, 0.000000000000000000, 1.000000000000000000 ) ) ;
#7878 = CARTESIAN_POINT ( 'NONE',  ( -5.000000000000001776, 5.000000000000001776, -105.9999999999999858 ) ) ;
#7879 = PRODUCT_DEFINITION ( 'UNKNOWN', '', #5437, #3254 ) ;
#7880 = PLANE ( 'NONE',  #8013 ) ;
#7881 = VECTOR ( 'NONE', #7223, 1000.000000000000000 ) ;
#7882 = CARTESIAN_POINT ( 'NONE',  ( 88.00000000000000000, -25.00000000000000000, -121.8314250403154659 ) ) ;
#7883 = ORIENTED_EDGE ( 'NONE', *, *, #7451, .T. ) ;
#7884 =( NAMED_UNIT ( * ) PLANE_ANGLE_UNIT ( ) SI_UNIT ( $, .RADIAN. ) );
#7885 = VERTEX_POINT ( 'NONE', #670 ) ;
#7886 = FACE_OUTER_BOUND ( 'NONE', #7253, .T. ) ;
#7887 = CARTESIAN_POINT ( 'NONE',  ( 259.0000000000000000, 5.000000000000001776, 139.9990000000000236 ) ) ;
#7888 = CIRCLE ( 'NONE', #3030, 2.649999999999987477 ) ;
#7889 = FACE_BOUND ( 'NONE', #4414, .T. ) ;
#7890 = CARTESIAN_POINT ( 'NONE',  ( -4.000000000000004441, 2.309401076758496263, -3.504269196027523847 ) ) ;
#7891 = FILL_AREA_STYLE ('',( #7153 ) ) ;
#7892 = DIRECTION ( 'NONE',  ( 1.000000000000000000, -1.734723475976806848E-16, 0.000000000000000000 ) ) ;
#7893 = B_SPLINE_CURVE_WITH_KNOTS ( 'NONE', 3,
 ( #7437, #3525, #5429, #6078, #1608, #1435, #869, #2911 ),
 .UNSPECIFIED., .F., .F.,
 ( 4, 2, 2, 4 ),
 ( 7.780516681398759253E-20, 0.002450665683189819696, 0.003675998524784729327, 0.004901331366379639391 ),
 .UNSPECIFIED. ) ;
#7894 = LINE ( 'NONE', #1898, #4924 ) ;
#7895 = ADVANCED_FACE ( 'NONE', ( #8598 ), #2416, .T. ) ;
#7896 = CARTESIAN_POINT ( 'NONE',  ( -5.000000000000001776, 5.000000000000001776, 148.0000000000000284 ) ) ;
#7897 = EDGE_CURVE ( 'NONE', #6418, #6181, #6284, .T. ) ;
#7898 = CARTESIAN_POINT ( 'NONE',  ( -10.00000000000000000, 1.224646799147353256E-15, -77.99999999999997158 ) ) ;
#7899 = EDGE_CURVE ( 'NONE', #4789, #8592, #5152, .T. ) ;
#7900 = CARTESIAN_POINT ( 'NONE',  ( -5.000000000000001776, 5.000000000000001776, -71.99999999999998579 ) ) ;
#7901 = SURFACE_STYLE_USAGE ( .BOTH. , #5971 ) ;
#7902 = AXIS2_PLACEMENT_3D ( 'NONE', #4315, #5744, #1137 ) ;
#7903 = VERTEX_POINT ( 'NONE', #3327 ) ;
#7904 = PLANE ( 'NONE',  #1071 ) ;
#7905 = ITEM_DEFINED_TRANSFORMATION ( 'NONE', 'NONE', #1142,  #594 ) ;
#7906 = ORIENTED_EDGE ( 'NONE', *, *, #794, .F. ) ;
#7907 = LINE ( 'NONE', #2520, #6592 ) ;
#7908 = LINE ( 'NONE', #3866, #4490 ) ;
#7909 = CIRCLE ( 'NONE', #390, 20.00000000000000000 ) ;
#7910 = CARTESIAN_POINT ( 'NONE',  ( 25.00000000000000000, 0.000000000000000000, 0.000000000000000000 ) ) ;
#7911 = ORIENTED_EDGE ( 'NONE', *, *, #5446, .T. ) ;
#7912 = DIRECTION ( 'NONE',  ( 1.000000000000000000, 0.000000000000000000, 0.000000000000000000 ) ) ;
#7913 = EDGE_CURVE ( 'NONE', #5372, #3043, #1899, .T. ) ;
#7914 = AXIS2_PLACEMENT_3D ( 'NONE', #4094, #7576, #6737 ) ;
#7915 = DIRECTION ( 'NONE',  ( -0.9227396241299338220, 0.000000000000000000, -0.3854239043709521972 ) ) ;
#7916 = LINE ( 'NONE', #1958, #8378 ) ;
#7917 = ORIENTED_EDGE ( 'NONE', *, *, #4495, .T. ) ;
#7918 = ORIENTED_EDGE ( 'NONE', *, *, #4897, .T. ) ;
#7919 = DIRECTION ( 'NONE',  ( -0.000000000000000000, -0.000000000000000000, 1.000000000000000000 ) ) ;
#7920 = CARTESIAN_POINT ( 'NONE',  ( 2.500000000000000000, 0.000000000000000000, 0.000000000000000000 ) ) ;
#7921 = APPLICATION_CONTEXT ( 'automotive_design' ) ;
#7922 = AXIS2_PLACEMENT_3D ( 'NONE', #7984, #620, #8030 ) ;
#7923 = DIRECTION ( 'NONE',  ( -1.000000000000000000, 0.000000000000000000, 0.000000000000000000 ) ) ;
#7924 = LINE ( 'NONE', #31, #2365 ) ;
#7925 = ORIENTED_EDGE ( 'NONE', *, *, #1589, .T. ) ;
#7926 = EDGE_CURVE ( 'NONE', #3184, #7335, #8245, .T. ) ;
#7927 =( NAMED_UNIT ( * ) SI_UNIT ( $, .STERADIAN. ) SOLID_ANGLE_UNIT ( ) );
#7928 = EDGE_CURVE ( 'NONE', #3529, #5237, #6092, .T. ) ;
#7929 = ORIENTED_EDGE ( 'NONE', *, *, #4168, .F. ) ;
#7930 = AXIS2_PLACEMENT_3D ( 'NONE', #91, #6011, #4024 ) ;
#7931 = CARTESIAN_POINT ( 'NONE',  ( 303.3333333333333144, -25.00000000000000000, 162.5000000000000853 ) ) ;
#7932 = EDGE_CURVE ( 'NONE', #798, #2080, #7125, .T. ) ;
#7933 = FACE_OUTER_BOUND ( 'NONE', #2352, .T. ) ;
#7934 = CARTESIAN_POINT ( 'NONE',  ( 2.500000000000000000, 2.357898499370433054, -1.951563910473907981E-15 ) ) ;
#7935 = ORIENTED_EDGE ( 'NONE', *, *, #1839, .T. ) ;
#7936 = DIRECTION ( 'NONE',  ( 0.000000000000000000, 0.000000000000000000, 1.000000000000000000 ) ) ;
#7937 =( NAMED_UNIT ( * ) SI_UNIT ( $, .STERADIAN. ) SOLID_ANGLE_UNIT ( ) );
#7938 = UNCERTAINTY_MEASURE_WITH_UNIT (LENGTH_MEASURE( 1.000000000000000082E-05 ), #3931, 'distance_accuracy_value', 'NONE');
#7939 = CARTESIAN_POINT ( 'NONE',  ( 0.000000000000000000, -25.00000000000000000, -157.5000000000000284 ) ) ;
#7940 = PLANE ( 'NONE',  #5190 ) ;
#7941 = LINE ( 'NONE', #3940, #6000 ) ;
#7942 = LINE ( 'NONE', #5406, #5825 ) ;
#7943 = DIRECTION ( 'NONE',  ( 0.000000000000000000, 0.000000000000000000, 1.000000000000000000 ) ) ;
#7944 = DIRECTION ( 'NONE',  ( 0.000000000000000000, 0.000000000000000000, 1.000000000000000000 ) ) ;
#7945 = ORIENTED_EDGE ( 'NONE', *, *, #121, .F. ) ;
#7946 = ORIENTED_EDGE ( 'NONE', *, *, #4096, .F. ) ;
#7947 = CONTEXT_DEPENDENT_SHAPE_REPRESENTATION ( #3148, #2953 ) ;
#7948 = ORIENTED_EDGE ( 'NONE', *, *, #5736, .T. ) ;
#7949 = LINE ( 'NONE', #545, #48 ) ;
#7950 = ADVANCED_FACE ( 'NONE', ( #5404 ), #4713, .F. ) ;
#7951 = DIRECTION ( 'NONE',  ( -0.000000000000000000, 1.000000000000000000, -0.000000000000000000 ) ) ;
#7952 = AXIS2_PLACEMENT_3D ( 'NONE', #7961, #1957, #5209 ) ;
#7953 = PRODUCT ( 'roller axis assy_r1', 'roller axis assy_r1', '', ( #1425 ) ) ;
#7954 = VECTOR ( 'NONE', #3811, 1000.000000000000000 ) ;
#7955 = DIRECTION ( 'NONE',  ( 1.000000000000000000, 0.000000000000000000, 0.000000000000000000 ) ) ;
#7956 = VERTEX_POINT ( 'NONE', #5447 ) ;
#7957 = LINE ( 'NONE', #553, #6290 ) ;
#7958 = DIRECTION ( 'NONE',  ( 0.000000000000000000, 1.000000000000000000, 0.000000000000000000 ) ) ;
#7959 = CARTESIAN_POINT ( 'NONE',  ( -20.00000000000000000, 2.449293598294706513E-15, -191.5685424949238325 ) ) ;
#7960 = EDGE_CURVE ( 'NONE', #3209, #4134, #1449, .T. ) ;
#7961 = CARTESIAN_POINT ( 'NONE',  ( 263.9999999999999432, -9.999999999999994671, -51.43142504031547446 ) ) ;
#7962 = CYLINDRICAL_SURFACE ( 'NONE', #3091, 2.649999999999985700 ) ;
#7963 = ORIENTED_EDGE ( 'NONE', *, *, #2896, .F. ) ;
#7964 = VECTOR ( 'NONE', #4974, 1000.000000000000114 ) ;
#7965 = ORIENTED_EDGE ( 'NONE', *, *, #7126, .F. ) ;
#7966 = DIRECTION ( 'NONE',  ( 1.000000000000000000, 0.000000000000000000, 0.000000000000000000 ) ) ;
#7967 = CARTESIAN_POINT ( 'NONE',  ( 10.00000000000000000, 0.000000000000000000, 7.000000000000006217 ) ) ;
#7968 = AXIS2_PLACEMENT_3D ( 'NONE', #4277, #7016, #1718 ) ;
#7969 = VECTOR ( 'NONE', #7975, 1000.000000000000000 ) ;
#7970 = CARTESIAN_POINT ( 'NONE',  ( 4.000000000001088907, 1.658577278524410170, -3.531553309554541720 ) ) ;
#7971 = DIRECTION ( 'NONE',  ( 0.000000000000000000, 0.000000000000000000, 1.000000000000000000 ) ) ;
#7972 = VERTEX_POINT ( 'NONE', #45 ) ;
#7973 = AXIS2_PLACEMENT_3D ( 'NONE', #2859, #6812, #1422 ) ;
#7974 = ORIENTED_EDGE ( 'NONE', *, *, #934, .F. ) ;
#7975 = DIRECTION ( 'NONE',  ( -0.000000000000000000, 1.000000000000000000, -0.000000000000000000 ) ) ;
#7976 = CIRCLE ( 'NONE', #4624, 2.649999999999985700 ) ;
#7977 = CIRCLE ( 'NONE', #4220, 2.500000000000000888 ) ;
#7978 = COLOUR_RGB ( '',1.000000000000000000, 0.9490196078431372140, 0.9098039215686274384 ) ;
#7979 = EDGE_CURVE ( 'NONE', #6518, #6809, #7368, .T. ) ;
#7980 = EDGE_CURVE ( 'NONE', #4658, #5548, #6053, .T. ) ;
#7981 = DIRECTION ( 'NONE',  ( -1.000000000000000000, 0.000000000000000000, -0.000000000000000000 ) ) ;
#7982 = CARTESIAN_POINT ( 'NONE',  ( 439.9999999999999432, -20.00000000000000000, 21.61857495968444454 ) ) ;
#7983 = VERTEX_POINT ( 'NONE', #221 ) ;
#7984 = CARTESIAN_POINT ( 'NONE',  ( 0.000000000000000000, 0.000000000000000000, 40.00000000000000000 ) ) ;
#7985 = AXIS2_PLACEMENT_3D ( 'NONE', #1594, #942, #2298 ) ;
#7986 = DIRECTION ( 'NONE',  ( -1.734723475976807341E-16, 1.000000000000000000, 0.000000000000000000 ) ) ;
#7987 = DIRECTION ( 'NONE',  ( -1.000000000000000000, -0.000000000000000000, -0.000000000000000000 ) ) ;
#7988 = CARTESIAN_POINT ( 'NONE',  ( 347.0000000000000000, -4.999999999999998224, 139.9990000000000236 ) ) ;
#7989 = AXIS2_PLACEMENT_3D ( 'NONE', #7878, #8012, #4647 ) ;
#7990 = FACE_OUTER_BOUND ( 'NONE', #192, .T. ) ;
#7991 = EDGE_CURVE ( 'NONE', #1525, #243, #4145, .T. ) ;
#7992 = DIRECTION ( 'NONE',  ( 0.000000000000000000, 0.000000000000000000, -1.000000000000000000 ) ) ;
#7993 = SHAPE_REPRESENTATION ( 'side rail', ( #594 ), #2832 ) ;
#7994 = EDGE_LOOP ( 'NONE', ( #4056, #3859 ) ) ;
#7995 = SHAPE_DEFINITION_REPRESENTATION ( #574, #3312 ) ;
#7996 = ORIENTED_EDGE ( 'NONE', *, *, #8088, .F. ) ;
#7997 = UNCERTAINTY_MEASURE_WITH_UNIT (LENGTH_MEASURE( 1.000000000000000082E-05 ), #4947, 'distance_accuracy_value', 'NONE');
#7998 = ORIENTED_EDGE ( 'NONE', *, *, #4213, .T. ) ;
#7999 = CARTESIAN_POINT ( 'NONE',  ( -5.000000000000001776, 5.000000000000001776, -71.99999999999998579 ) ) ;
#8000 = CIRCLE ( 'NONE', #196, 2.649999999999985700 ) ;
#8001 = DIRECTION ( 'NONE',  ( -1.734723475976807587E-16, 0.000000000000000000, 1.000000000000000000 ) ) ;
#8002 = ORIENTED_EDGE ( 'NONE', *, *, #3808, .F. ) ;
#8003 = LINE ( 'NONE', #3339, #5087 ) ;
#8004 = ORIENTED_EDGE ( 'NONE', *, *, #5738, .F. ) ;
#8005 = CARTESIAN_POINT ( 'NONE',  ( 136.6666666666666288, -25.00000000000000000, 162.5000000000000853 ) ) ;
#8006 = CARTESIAN_POINT ( 'NONE',  ( 386.6666666666666288, -20.00000000000000000, 165.1500000000000625 ) ) ;
#8007 = CARTESIAN_POINT ( 'NONE',  ( 352.0000000000000000, -9.999999999999998224, -16.23142504031548228 ) ) ;
#8008 = CARTESIAN_POINT ( 'NONE',  ( -5.000000000000000000, -5.000000000000000000, 148.0000000000000284 ) ) ;
#8009 = ORIENTED_EDGE ( 'NONE', *, *, #7696, .F. ) ;
#8010 = ORIENTED_EDGE ( 'NONE', *, *, #5126, .T. ) ;
#8011 = DIRECTION ( 'NONE',  ( -1.000000000000000000, 0.000000000000000000, 0.000000000000000000 ) ) ;
#8012 = DIRECTION ( 'NONE',  ( -1.734723475976806848E-16, -1.000000000000000000, 0.000000000000000000 ) ) ;
#8013 = AXIS2_PLACEMENT_3D ( 'NONE', #4007, #7923, #1343 ) ;
#8014 = ADVANCED_FACE ( 'NONE', ( #2151 ), #4060, .F. ) ;
#8015 = VECTOR ( 'NONE', #5032, 1000.000000000000000 ) ;
#8016 = EDGE_CURVE ( 'NONE', #2428, #832, #8206, .T. ) ;
#8017 = CARTESIAN_POINT ( 'NONE',  ( 5.000000000000000000, 5.000000000000000000, -27.99999999999999645 ) ) ;
#8018 = DIRECTION ( 'NONE',  ( -0.000000000000000000, 1.000000000000000000, -0.000000000000000000 ) ) ;
#8019 = VERTEX_POINT ( 'NONE', #6754 ) ;
#8020 = EDGE_CURVE ( 'NONE', #5053, #7465, #1403, .T. ) ;
#8021 = AXIS2_PLACEMENT_3D ( 'NONE', #5936, #8569, #7295 ) ;
#8022 = B_SPLINE_CURVE_WITH_KNOTS ( 'NONE', 3,
 ( #2243, #3071, #3681, #4854, #2385, #6326, #6853, #364 ),
 .UNSPECIFIED., .F., .F.,
 ( 4, 2, 2, 4 ),
 ( 2.465131517071610173E-07, 0.001183067374689837636, 0.001774477805458902699, 0.002365888236227967761 ),
 .UNSPECIFIED. ) ;
#8023 = ORIENTED_EDGE ( 'NONE', *, *, #338, .F. ) ;
#8024 = DIRECTION ( 'NONE',  ( 0.000000000000000000, 0.000000000000000000, 1.000000000000000000 ) ) ;
#8025 = AXIS2_PLACEMENT_3D ( 'NONE', #5538, #131, #2801 ) ;
#8026 = CIRCLE ( 'NONE', #511, 2.649999999999985700 ) ;
#8027 = CARTESIAN_POINT ( 'NONE',  ( -5.000000000000000000, -5.000000000000000000, 148.0000000000000284 ) ) ;
#8028 = LINE ( 'NONE', #2063, #959 ) ;
#8029 = ORIENTED_EDGE ( 'NONE', *, *, #8469, .T. ) ;
#8030 = DIRECTION ( 'NONE',  ( -1.000000000000000000, 0.000000000000000000, -0.000000000000000000 ) ) ;
#8031 = CIRCLE ( 'NONE', #3575, 2.649999999999985700 ) ;
#8032 = ADVANCED_FACE ( 'NONE', ( #8162 ), #6707, .T. ) ;
#8033 = AXIS2_PLACEMENT_3D ( 'NONE', #6179, #2879, #2230 ) ;
#8034 = PRODUCT ( 'base plate', 'base plate', '', ( #1512 ) ) ;
#8035 = FACE_OUTER_BOUND ( 'NONE', #5823, .T. ) ;
#8036 = DIRECTION ( 'NONE',  ( 1.000000000000000000, 0.000000000000000000, 0.000000000000000000 ) ) ;
#8037 = DIRECTION ( 'NONE',  ( -0.000000000000000000, 1.000000000000000000, -0.000000000000000000 ) ) ;
#8038 = DIRECTION ( 'NONE',  ( -0.000000000000000000, -0.000000000000000000, 1.000000000000000000 ) ) ;
#8039 = CARTESIAN_POINT ( 'NONE',  ( 4.000000000000000000, 0.000000000000000000, 0.000000000000000000 ) ) ;
#8040 = EDGE_LOOP ( 'NONE', ( #6595, #5478 ) ) ;
#8041 = EDGE_LOOP ( 'NONE', ( #611, #3048, #6217, #1507 ) ) ;
#8042 = VECTOR ( 'NONE', #4657, 1000.000000000000000 ) ;
#8043 = ORIENTED_EDGE ( 'NONE', *, *, #7246, .F. ) ;
#8044 = LINE ( 'NONE', #769, #4588 ) ;
#8045 = PRODUCT_RELATED_PRODUCT_CATEGORY ( 'part', '', ( #7393 ) ) ;
#8046 = DIRECTION ( 'NONE',  ( 1.734723475976807587E-16, 1.000000000000000000, 0.000000000000000000 ) ) ;
#8047 = ORIENTED_EDGE ( 'NONE', *, *, #1007, .F. ) ;
#8048 = DIRECTION ( 'NONE',  ( 0.000000000000000000, -0.8660254037844390407, -0.4999999999999994449 ) ) ;
#8049 = VERTEX_POINT ( 'NONE', #5362 ) ;
#8050 = CARTESIAN_POINT ( 'NONE',  ( 5.000000000000000000, 5.000000000000000000, 42.00000000000000711 ) ) ;
#8051 = DIRECTION ( 'NONE',  ( 1.000000000000000000, 0.000000000000000000, 0.000000000000000000 ) ) ;
#8052 = ITEM_DEFINED_TRANSFORMATION ( 'NONE', 'NONE', #568,  #594 ) ;
#8053 = FILL_AREA_STYLE ('',( #2211 ) ) ;
#8054 = ORIENTED_EDGE ( 'NONE', *, *, #2628, .F. ) ;
#8055 = ORIENTED_EDGE ( 'NONE', *, *, #8227, .F. ) ;
#8056 = DIRECTION ( 'NONE',  ( -0.000000000000000000, -0.000000000000000000, -1.000000000000000000 ) ) ;
#8057 = VECTOR ( 'NONE', #738, 1000.000000000000000 ) ;
#8058 = CARTESIAN_POINT ( 'NONE',  ( -5.000000000000000000, -5.000000000000000000, 148.0000000000000284 ) ) ;
#8059 = EDGE_CURVE ( 'NONE', #1635, #4789, #4755, .T. ) ;
#8060 = CARTESIAN_POINT ( 'NONE',  ( 4.203935335434060505, 1.640780671294165272, -3.598452447879202598 ) ) ;
#8061 = VECTOR ( 'NONE', #711, 1000.000000000000000 ) ;
#8062 = CARTESIAN_POINT ( 'NONE',  ( 20.00000000000000000, 0.000000000000000000, 120.0000000000000142 ) ) ;
#8063 = EDGE_LOOP ( 'NONE', ( #6306, #3487, #5400, #8029 ) ) ;
#8064 = EDGE_CURVE ( 'NONE', #8324, #1841, #160, .T. ) ;
#8065 = FILL_AREA_STYLE ('',( #3970 ) ) ;
#8066 = LINE ( 'NONE', #6081, #2117 ) ;
#8067 = ORIENTED_EDGE ( 'NONE', *, *, #8202, .F. ) ;
#8068 = VERTEX_POINT ( 'NONE', #1540 ) ;
#8069 = CARTESIAN_POINT ( 'NONE',  ( -4.999999999999998224, 140.0000000000000000, 15.00000000000000355 ) ) ;
#8070 = EDGE_CURVE ( 'NONE', #35, #3680, #6185, .T. ) ;
#8071 = AXIS2_PLACEMENT_3D ( 'NONE', #4889, #3500, #6322 ) ;
#8072 = EDGE_CURVE ( 'NONE', #1399, #8107, #2678, .T. ) ;
#8073 = DIRECTION ( 'NONE',  ( 0.000000000000000000, 0.000000000000000000, -1.000000000000000000 ) ) ;
#8074 = FACE_OUTER_BOUND ( 'NONE', #5974, .T. ) ;
#8075 = EDGE_LOOP ( 'NONE', ( #1971, #5915, #6801, #7998 ) ) ;
#8076 = DIRECTION ( 'NONE',  ( 0.000000000000000000, -0.000000000000000000, 1.000000000000000000 ) ) ;
#8077 = CIRCLE ( 'NONE', #7930, 2.100000000000000089 ) ;
#8078 = CYLINDRICAL_SURFACE ( 'NONE', #6843, 2.649999999999985700 ) ;
#8079 = CARTESIAN_POINT ( 'NONE',  ( -5.000000000000000000, -5.000000000000000000, 140.0000000000000000 ) ) ;
#8080 = CARTESIAN_POINT ( 'NONE',  ( 5.000000000000000000, 5.000000000000000000, 148.0000000000000284 ) ) ;
#8081 = DIRECTION ( 'NONE',  ( -1.000000000000000000, 0.000000000000000000, 0.000000000000000000 ) ) ;
#8082 = LINE ( 'NONE', #182, #5365 ) ;
#8083 = ORIENTED_EDGE ( 'NONE', *, *, #4920, .T. ) ;
#8084 = ORIENTED_EDGE ( 'NONE', *, *, #5041, .F. ) ;
#8085 = VERTEX_POINT ( 'NONE', #888 ) ;
#8086 = DIRECTION ( 'NONE',  ( 1.000000000000000000, 0.000000000000000000, 0.000000000000000000 ) ) ;
#8087 = PRESENTATION_STYLE_ASSIGNMENT (( #1414 ) ) ;
#8088 = EDGE_CURVE ( 'NONE', #3290, #628, #2237, .T. ) ;
#8089 = AXIS2_PLACEMENT_3D ( 'NONE', #8453, #8363, #7001 ) ;
#8090 = EDGE_CURVE ( 'NONE', #5141, #1878, #8249, .T. ) ;
#8091 = ORIENTED_EDGE ( 'NONE', *, *, #2603, .F. ) ;
#8092 = FACE_OUTER_BOUND ( 'NONE', #3736, .T. ) ;
#8093 = ORIENTED_EDGE ( 'NONE', *, *, #5606, .T. ) ;
#8094 = CARTESIAN_POINT ( 'NONE',  ( 5.000000000000000000, -5.000000000000000000, 148.0000000000000284 ) ) ;
#8095 = APPLICATION_CONTEXT ( 'automotive_design' ) ;
#8096 = DIRECTION ( 'NONE',  ( -1.000000000000000000, 0.000000000000000000, 0.000000000000000000 ) ) ;
#8097 = FACE_OUTER_BOUND ( 'NONE', #1266, .T. ) ;
#8098 = VERTEX_POINT ( 'NONE', #266 ) ;
#8099 = EDGE_LOOP ( 'NONE', ( #5937, #7946, #4328, #113 ) ) ;
#8100 = CARTESIAN_POINT ( 'NONE',  ( 53.33333333333330017, -14.99999999999999822, 162.5000000000000853 ) ) ;
#8101 = CARTESIAN_POINT ( 'NONE',  ( -4.000000000000000888, -2.309401076758512694, -3.504269196027526512 ) ) ;
#8102 = CARTESIAN_POINT ( 'NONE',  ( 0.000000000000000000, 0.000000000000000000, 0.000000000000000000 ) ) ;
#8103 = DIRECTION ( 'NONE',  ( -1.000000000000000000, 0.000000000000000000, -0.000000000000000000 ) ) ;
#8104 = PRODUCT ( 'roller axis assy_r3', 'roller axis assy_r3', '', ( #6597 ) ) ;
#8105 = PLANE ( 'NONE',  #7914 ) ;
#8106 = ADVANCED_FACE ( 'NONE', ( #8379 ), #3622, .F. ) ;
#8107 = VERTEX_POINT ( 'NONE', #2929 ) ;
#8108 = COLOUR_RGB ( '',0.8941176470588234615, 0.8941176470588234615, 0.8941176470588234615 ) ;
#8109 = FILL_AREA_STYLE_COLOUR ( '', #4679 ) ;
#8110 = DIRECTION ( 'NONE',  ( 1.000000000000000000, 0.000000000000000000, 0.000000000000000000 ) ) ;
#8111 = CARTESIAN_POINT ( 'NONE',  ( 0.2500000000000002220, 5.204748896376250699E-16, -4.250000000000000000 ) ) ;
#8112 = ORIENTED_EDGE ( 'NONE', *, *, #5397, .F. ) ;
#8113 = AXIS2_PLACEMENT_3D ( 'NONE', #4932, #5705, #2422 ) ;
#8114 = DIRECTION ( 'NONE',  ( -0.000000000000000000, -0.000000000000000000, 1.000000000000000000 ) ) ;
#8115 = CIRCLE ( 'NONE', #1566, 10.00000000000000000 ) ;
#8116 = FACE_OUTER_BOUND ( 'NONE', #7837, .T. ) ;
#8117 = DIRECTION ( 'NONE',  ( 0.000000000000000000, -0.000000000000000000, 1.000000000000000000 ) ) ;
#8118 = VERTEX_POINT ( 'NONE', #7593 ) ;
#8119 = FACE_BOUND ( 'NONE', #4037, .T. ) ;
#8120 = AXIS2_PLACEMENT_3D ( 'NONE', #3884, #4608, #1260 ) ;
#8121 = CARTESIAN_POINT ( 'NONE',  ( -5.000000000000001776, 5.000000000000001776, -36.00000000000000000 ) ) ;
#8122 = DIRECTION ( 'NONE',  ( -0.000000000000000000, -0.000000000000000000, -1.000000000000000000 ) ) ;
#8123 = LINE ( 'NONE', #4933, #5005 ) ;
#8124 = ADVANCED_FACE ( 'NONE', ( #5622 ), #8337, .F. ) ;
#8125 = LINE ( 'NONE', #763, #2771 ) ;
#8126 = DIRECTION ( 'NONE',  ( -1.000000000000000000, 0.000000000000000000, 0.000000000000000000 ) ) ;
#8127 = VECTOR ( 'NONE', #669, 1000.000000000000000 ) ;
#8128 = ORIENTED_EDGE ( 'NONE', *, *, #6796, .T. ) ;
#8129 = EDGE_CURVE ( 'NONE', #3441, #243, #4236, .T. ) ;
#8130 = ORIENTED_EDGE ( 'NONE', *, *, #400, .T. ) ;
#8131 = VERTEX_POINT ( 'NONE', #6969 ) ;
#8132 = DIRECTION ( 'NONE',  ( 0.000000000000000000, 0.000000000000000000, -1.000000000000000000 ) ) ;
#8133 = CARTESIAN_POINT ( 'NONE',  ( -20.00000000000000000, 135.0000000000000000, 0.000000000000000000 ) ) ;
#8134 = VECTOR ( 'NONE', #5697, 1000.000000000000000 ) ;
#8135 = ORIENTED_EDGE ( 'NONE', *, *, #1315, .T. ) ;
#8136 = DIRECTION ( 'NONE',  ( -1.000000000000000000, 0.000000000000000000, 0.000000000000000000 ) ) ;
#8137 = ORIENTED_EDGE ( 'NONE', *, *, #8436, .F. ) ;
#8138 = CYLINDRICAL_SURFACE ( 'NONE', #4911, 10.00000000000000000 ) ;
#8139 = DIRECTION ( 'NONE',  ( 1.734723475976807587E-16, 1.000000000000000000, 0.000000000000000000 ) ) ;
#8140 = DIRECTION ( 'NONE',  ( -0.000000000000000000, 1.000000000000000000, -0.000000000000000000 ) ) ;
#8141 = VERTEX_POINT ( 'NONE', #6926 ) ;
#8142 = VERTEX_POINT ( 'NONE', #4367 ) ;
#8143 = ADVANCED_FACE ( 'NONE', ( #1629, #6231 ), #6887, .T. ) ;
#8144 = CARTESIAN_POINT ( 'NONE',  ( 352.0000000000000000, -20.00000000000000000, -18.88142504031545243 ) ) ;
#8145 = CARTESIAN_POINT ( 'NONE',  ( 1.567478505476134606E-15, 4.618802153517012066, -3.433295621305382905 ) ) ;
#8146 = LINE ( 'NONE', #1472, #3161 ) ;
#8147 = CARTESIAN_POINT ( 'NONE',  ( 0.000000000000000000, 0.000000000000000000, -27.99999999999999645 ) ) ;
#8148 = EDGE_LOOP ( 'NONE', ( #1777, #4436 ) ) ;
#8149 = DIRECTION ( 'NONE',  ( -0.000000000000000000, -0.000000000000000000, 1.000000000000000000 ) ) ;
#8150 = CARTESIAN_POINT ( 'NONE',  ( -4.197393957002303999, -7.773935952363655451E-14, -3.503767560748929810 ) ) ;
#8151 = ORIENTED_EDGE ( 'NONE', *, *, #3282, .T. ) ;
#8152 = LINE ( 'NONE', #7488, #1019 ) ;
#8153 = FACE_BOUND ( 'NONE', #6439, .T. ) ;
#8154 = AXIS2_PLACEMENT_3D ( 'NONE', #7112, #1818, #3725 ) ;
#8155 = FACE_OUTER_BOUND ( 'NONE', #4719, .T. ) ;
#8156 = CARTESIAN_POINT ( 'NONE',  ( 88.00000000000000000, -20.00000000000000000, -124.4814250403154574 ) ) ;
#8157 = ORIENTED_EDGE ( 'NONE', *, *, #8016, .T. ) ;
#8158 = CARTESIAN_POINT ( 'NONE',  ( 2.649999999999987477, 157.5000000000000284, 5.000000000000000888 ) ) ;
#8159 = FACE_OUTER_BOUND ( 'NONE', #2795, .T. ) ;
#8160 = CIRCLE ( 'NONE', #6756, 2.649999999999985700 ) ;
#8161 = VECTOR ( 'NONE', #4383, 1000.000000000000114 ) ;
#8162 = FACE_OUTER_BOUND ( 'NONE', #325, .T. ) ;
#8163 = DIRECTION ( 'NONE',  ( -0.000000000000000000, -0.000000000000000000, 1.000000000000000000 ) ) ;
#8164=STYLED_ITEM('',(#8657),#2129);
#8165 = CARTESIAN_POINT ( 'NONE',  ( -1.274258131565027874, -3.883108878240886241, -3.220599429844051009 ) ) ;
#8166 = LINE ( 'NONE', #4761, #7455 ) ;
#8167 = AXIS2_PLACEMENT_3D ( 'NONE', #7535, #4926, #4966 ) ;
#8168 = ORIENTED_EDGE ( 'NONE', *, *, #776, .F. ) ;
#8169 = VERTEX_POINT ( 'NONE', #973 ) ;
#8170 = ADVANCED_FACE ( 'NONE', ( #6274 ), #1012, .T. ) ;
#8171 = VERTEX_POINT ( 'NONE', #3671 ) ;
#8172 = CARTESIAN_POINT ( 'NONE',  ( -10.00000000000000000, 1.224646799147353256E-15, -63.99999999999997158 ) ) ;
#8173 = ADVANCED_FACE ( 'NONE', ( #5573 ), #8295, .T. ) ;
#8174 =( NAMED_UNIT ( * ) PLANE_ANGLE_UNIT ( ) SI_UNIT ( $, .RADIAN. ) );
#8175 = PRODUCT_DEFINITION_SHAPE ( 'NONE', 'NONE',  #3515 ) ;
#8176 = ADVANCED_FACE ( 'NONE', ( #353 ), #3021, .T. ) ;
#8177 = ORIENTED_EDGE ( 'NONE', *, *, #2829, .T. ) ;
#8178 = CARTESIAN_POINT ( 'NONE',  ( 170.9999999999999716, -4.999999999999998224, 139.9990000000000236 ) ) ;
#8179 = ORIENTED_EDGE ( 'NONE', *, *, #8498, .F. ) ;
#8180 = CARTESIAN_POINT ( 'NONE',  ( 0.6937372685066666156, -4.453844082567737672, -3.610536846335894445 ) ) ;
#8181 = CARTESIAN_POINT ( 'NONE',  ( -5.000000000000001776, 5.000000000000001776, 140.0000000000000000 ) ) ;
#8182 = CARTESIAN_POINT ( 'NONE',  ( 20.00000000000000000, 140.0000000000000000, 40.00000000000000000 ) ) ;
#8183 = ORIENTED_EDGE ( 'NONE', *, *, #5522, .T. ) ;
#8184 = ORIENTED_EDGE ( 'NONE', *, *, #3163, .T. ) ;
#8185 = DIRECTION ( 'NONE',  ( 0.000000000000000000, 0.000000000000000000, 1.000000000000000000 ) ) ;
#8186 = DIRECTION ( 'NONE',  ( 0.000000000000000000, 0.000000000000000000, 1.000000000000000000 ) ) ;
#8187 = CARTESIAN_POINT ( 'NONE',  ( -4.000000000000000000, 2.309401076758498483, -0.4999999999999927280 ) ) ;
#8188 = CARTESIAN_POINT ( 'NONE',  ( -0.1750025118121544265, -4.719839900820635314, -3.469254087858253399 ) ) ;
#8189 = ORIENTED_EDGE ( 'NONE', *, *, #3224, .F. ) ;
#8190 = VECTOR ( 'NONE', #8242, 1000.000000000000000 ) ;
#8191 =( NAMED_UNIT ( * ) PLANE_ANGLE_UNIT ( ) SI_UNIT ( $, .RADIAN. ) );
#8192 = CARTESIAN_POINT ( 'NONE',  ( -4.197393957002303999, -0.8151795401431414234, -3.503767560748935139 ) ) ;
#8193 = EDGE_LOOP ( 'NONE', ( #4720, #1072, #5630 ) ) ;
#8194 = ORIENTED_EDGE ( 'NONE', *, *, #1276, .F. ) ;
#8195 = PLANE ( 'NONE',  #1433 ) ;
#8196 = FACE_BOUND ( 'NONE', #99, .T. ) ;
#8197 = AXIS2_PLACEMENT_3D ( 'NONE', #957, #785, #5477 ) ;
#8198 = CARTESIAN_POINT ( 'NONE',  ( 20.00000000000000000, 0.000000000000000000, -84.56854249492380404 ) ) ;
#8199 = ADVANCED_FACE ( 'NONE', ( #7682 ), #3065, .T. ) ;
#8200 = LINE ( 'NONE', #6225, #4428 ) ;
#8201 = ORIENTED_EDGE ( 'NONE', *, *, #1731, .T. ) ;
#8202 = EDGE_CURVE ( 'NONE', #1468, #2893, #3955, .T. ) ;
#8203 = CARTESIAN_POINT ( 'NONE',  ( -0.6937372685066653943, 4.453844082567723461, -3.610536846335889116 ) ) ;
#8204 = EDGE_CURVE ( 'NONE', #7049, #3816, #5036, .T. ) ;
#8205 = DIRECTION ( 'NONE',  ( 0.000000000000000000, 0.000000000000000000, 1.000000000000000000 ) ) ;
#8206 = LINE ( 'NONE', #3411, #4756 ) ;
#8207 =( REPRESENTATION_RELATIONSHIP ('NONE','NONE', #3312, #4754 ) REPRESENTATION_RELATIONSHIP_WITH_TRANSFORMATION ( #5510 )SHAPE_REPRESENTATION_RELATIONSHIP( ) );
#8208 = CIRCLE ( 'NONE', #4447, 2.649999999999985700 ) ;
#8209 = LINE ( 'NONE', #4187, #2088 ) ;
#8210 = LINE ( 'NONE', #936, #4161 ) ;
#8211 = DIRECTION ( 'NONE',  ( 0.000000000000000000, 1.000000000000000000, 0.000000000000000000 ) ) ;
#8213 = ORIENTED_EDGE ( 'NONE', *, *, #2628, .T. ) ;
#8212 = ADVANCED_FACE ( 'NONE', ( #6122 ), #3486, .T. ) ;
#8214 = ORIENTED_EDGE ( 'NONE', *, *, #525, .F. ) ;
#8215 = VERTEX_POINT ( 'NONE', #8111 ) ;
#8216 = CARTESIAN_POINT ( 'NONE',  ( 0.000000000000000000, 0.000000000000000000, 42.00000000000000711 ) ) ;
#8217 = VECTOR ( 'NONE', #3652, 1000.000000000000000 ) ;
#8218 = LINE ( 'NONE', #2855, #8532 ) ;
#8219 = ORIENTED_EDGE ( 'NONE', *, *, #3025, .F. ) ;
#8220 = DIRECTION ( 'NONE',  ( 0.000000000000000000, 0.000000000000000000, -1.000000000000000000 ) ) ;
#8221 = ORIENTED_EDGE ( 'NONE', *, *, #3084, .T. ) ;
#8222 = CARTESIAN_POINT ( 'NONE',  ( 0.000000000000000000, 0.000000000000000000, 42.00000000000000711 ) ) ;
#8223 = LINE ( 'NONE', #2306, #8161 ) ;
#8224 = SHAPE_DEFINITION_REPRESENTATION ( #3996, #2707 ) ;
#8225 = CARTESIAN_POINT ( 'NONE',  ( 0.000000000000000000, 0.000000000000000000, 120.0000000000000142 ) ) ;
#8226 = ORIENTED_EDGE ( 'NONE', *, *, #7960, .F. ) ;
#8227 = EDGE_CURVE ( 'NONE', #5985, #2939, #8066, .T. ) ;
#8228 = ORIENTED_EDGE ( 'NONE', *, *, #5738, .T. ) ;
#8229 = CARTESIAN_POINT ( 'NONE',  ( -5.000000000000000000, -5.000000000000000000, 148.0000000000000284 ) ) ;
#8230 = CARTESIAN_POINT ( 'NONE',  ( 5.000000000000000000, 5.000000000000000000, 148.0000000000000284 ) ) ;
#8231 = DIRECTION ( 'NONE',  ( 1.000000000000000000, 0.000000000000000000, 0.000000000000000000 ) ) ;
#8232 = CARTESIAN_POINT ( 'NONE',  ( 0.000000000000000000, 0.000000000000000000, 0.000000000000000000 ) ) ;
#8233 = ORIENTED_EDGE ( 'NONE', *, *, #121, .T. ) ;
#8234 =( GEOMETRIC_REPRESENTATION_CONTEXT ( 3 ) GLOBAL_UNCERTAINTY_ASSIGNED_CONTEXT ( ( #2388 ) ) GLOBAL_UNIT_ASSIGNED_CONTEXT ( ( #2179, #2272, #4221 ) ) REPRESENTATION_CONTEXT ( 'NONE', 'WORKASPACE' ) );
#8235 = DIRECTION ( 'NONE',  ( -0.000000000000000000, 0.000000000000000000, -1.000000000000000000 ) ) ;
#8236 = ADVANCED_FACE ( 'NONE', ( #2092 ), #1569, .F. ) ;
#8237 = ORIENTED_EDGE ( 'NONE', *, *, #5913, .T. ) ;
#8238 = DIRECTION ( 'NONE',  ( -0.000000000000000000, 1.000000000000000000, -0.000000000000000000 ) ) ;
#8239 = CARTESIAN_POINT ( 'NONE',  ( 303.3333333333333144, -14.99999999999999822, 162.5000000000000853 ) ) ;
#8240 = AXIS2_PLACEMENT_3D ( 'NONE', #3301, #1293, #7871 ) ;
#8241 = DIRECTION ( 'NONE',  ( -1.000000000000000000, -0.000000000000000000, -0.000000000000000000 ) ) ;
#8242 = DIRECTION ( 'NONE',  ( -0.000000000000000000, -1.000000000000000000, -0.000000000000000000 ) ) ;
#8243 = EDGE_LOOP ( 'NONE', ( #1817, #1056, #1668, #3206 ) ) ;
#8244 = CARTESIAN_POINT ( 'NONE',  ( -5.000000000000000000, -5.000000000000000000, -143.0000000000000284 ) ) ;
#8245 = CIRCLE ( 'NONE', #3794, 10.00000000000000000 ) ;
#8246 = DIRECTION ( 'NONE',  ( -1.000000000000000000, 0.000000000000000000, 0.000000000000000000 ) ) ;
#8247 = AXIS2_PLACEMENT_3D ( 'NONE', #3935, #3278, #7892 ) ;
#8248 = EDGE_CURVE ( 'NONE', #3592, #6335, #77, .T. ) ;
#8249 = LINE ( 'NONE', #5057, #5306 ) ;
#8250 = VECTOR ( 'NONE', #1464, 1000.000000000000000 ) ;
#8251 = CARTESIAN_POINT ( 'NONE',  ( 170.9999999999999716, 5.000000000000001776, 139.9990000000000236 ) ) ;
#8252 = AXIS2_PLACEMENT_3D ( 'NONE', #2709, #5351, #8024 ) ;
#8253 = DIRECTION ( 'NONE',  ( -0.000000000000000000, -0.000000000000000000, 1.000000000000000000 ) ) ;
#8254 = SURFACE_STYLE_FILL_AREA ( #7104 ) ;
#8255 = VERTEX_POINT ( 'NONE', #4875 ) ;
#8256 = VECTOR ( 'NONE', #5770, 1000.000000000000000 ) ;
#8257 = AXIS2_PLACEMENT_3D ( 'NONE', #1292, #3958, #6596 ) ;
#8258 = ORIENTED_EDGE ( 'NONE', *, *, #2851, .T. ) ;
#8259 = EDGE_LOOP ( 'NONE', ( #6823, #6288, #1737, #2901 ) ) ;
#8260 = DIRECTION ( 'NONE',  ( -1.734723475976806848E-16, 1.000000000000000000, 0.000000000000000000 ) ) ;
#8261 = DIRECTION ( 'NONE',  ( -0.000000000000000000, -0.000000000000000000, 1.000000000000000000 ) ) ;
#8262 = EDGE_CURVE ( 'NONE', #1426, #3213, #2180, .T. ) ;
#8263 = VECTOR ( 'NONE', #3764, 1000.000000000000000 ) ;
#8264 = ORIENTED_EDGE ( 'NONE', *, *, #6795, .F. ) ;
#8265 = DIRECTION ( 'NONE',  ( 1.224646799147353207E-16, 1.000000000000000000, 0.000000000000000000 ) ) ;
#8266 = ORIENTED_EDGE ( 'NONE', *, *, #7291, .F. ) ;
#8267 = CARTESIAN_POINT ( 'NONE',  ( -5.000000000000001776, 5.000000000000001776, -105.9999999999999858 ) ) ;
#8268 = CONTEXT_DEPENDENT_SHAPE_REPRESENTATION ( #922, #3033 ) ;
#8269 = LINE ( 'NONE', #2307, #7954 ) ;
#8270 = ORIENTED_EDGE ( 'NONE', *, *, #2407, .T. ) ;
#8271 = UNCERTAINTY_MEASURE_WITH_UNIT (LENGTH_MEASURE( 1.000000000000000082E-05 ), #2028, 'distance_accuracy_value', 'NONE');
#8272 = ORIENTED_EDGE ( 'NONE', *, *, #1652, .F. ) ;
#8273 = AXIS2_PLACEMENT_3D ( 'NONE', #7279, #5800, #4456 ) ;
#8274 = CARTESIAN_POINT ( 'NONE',  ( -30.00000000000000000, -15.00000000000000000, 145.0000000000000284 ) ) ;
#8275 = CARTESIAN_POINT ( 'NONE',  ( 2.290893957444128645E-15, 4.647089433458768681, -3.572167766733382877 ) ) ;
#8276 = VECTOR ( 'NONE', #1796, 1000.000000000000114 ) ;
#8277 = PLANE ( 'NONE',  #6045 ) ;
#8278 = DIRECTION ( 'NONE',  ( 0.000000000000000000, 0.000000000000000000, -1.000000000000000000 ) ) ;
#8279 = ORIENTED_EDGE ( 'NONE', *, *, #1454, .F. ) ;
#8280 = CARTESIAN_POINT ( 'NONE',  ( -30.00000000000002842, -20.00000000000000000, 200.0000000000000000 ) ) ;
#8281 = ORIENTED_EDGE ( 'NONE', *, *, #4284, .F. ) ;
#8282 = VERTEX_POINT ( 'NONE', #2833 ) ;
#8283 = ADVANCED_FACE ( 'NONE', ( #7486 ), #4788, .F. ) ;
#8284 = CARTESIAN_POINT ( 'NONE',  ( -4.000000000000000000, 2.309401076758498483, -0.4999999999999927280 ) ) ;
#8285 = FACE_BOUND ( 'NONE', #1325, .T. ) ;
#8286 = ADVANCED_FACE ( 'NONE', ( #4135 ), #2914, .F. ) ;
#8287 = EDGE_CURVE ( 'NONE', #3178, #5009, #7396, .T. ) ;
#8288 = CARTESIAN_POINT ( 'NONE',  ( 0.000000000000000000, 0.000000000000000000, 120.0000000000000142 ) ) ;
#8289 = CARTESIAN_POINT ( 'NONE',  ( -2.500000000000000888, 0.000000000000000000, -4.974599999999998801 ) ) ;
#8290 = EDGE_LOOP ( 'NONE', ( #8398, #8112 ) ) ;
#8291 = DIRECTION ( 'NONE',  ( 0.000000000000000000, -1.000000000000000000, 0.000000000000000000 ) ) ;
#8292 = APPLICATION_PROTOCOL_DEFINITION ( 'draft international standard', 'automotive_design', 1998, #6744 ) ;
#8293 = VECTOR ( 'NONE', #7615, 1000.000000000000000 ) ;
#8294 = CARTESIAN_POINT ( 'NONE',  ( -2.000000000000007550, -3.464101615137749945, 0.000000000000000000 ) ) ;
#8295 = PLANE ( 'NONE',  #7690 ) ;
#8296 = CIRCLE ( 'NONE', #209, 10.00000000000000000 ) ;
#8297 = FACE_OUTER_BOUND ( 'NONE', #4821, .T. ) ;
#8298 = CARTESIAN_POINT ( 'NONE',  ( 0.1756481739660539498, -4.720212674038995360, -3.469390959564070620 ) ) ;
#8299 = ADVANCED_FACE ( 'NONE', ( #1438 ), #7578, .F. ) ;
#8300 = ORIENTED_EDGE ( 'NONE', *, *, #1351, .F. ) ;
#8301 = AXIS2_PLACEMENT_3D ( 'NONE', #2162, #4815, #902 ) ;
#8302 = ORIENTED_EDGE ( 'NONE', *, *, #5570, .F. ) ;
#8303 = AXIS2_PLACEMENT_3D ( 'NONE', #3040, #3638, #6862 ) ;
#8304 = ORIENTED_EDGE ( 'NONE', *, *, #3239, .F. ) ;
#8305 = DIRECTION ( 'NONE',  ( -1.000000000000000000, -0.000000000000000000, -0.000000000000000000 ) ) ;
#8306 = LINE ( 'NONE', #6371, #2974 ) ;
#8307 = AXIS2_PLACEMENT_3D ( 'NONE', #5153, #6539, #6014 ) ;
#8308 = VECTOR ( 'NONE', #5657, 1000.000000000000114 ) ;
#8309 = EDGE_LOOP ( 'NONE', ( #4632, #2450, #8002, #2047 ) ) ;
#8310 = ORIENTED_EDGE ( 'NONE', *, *, #7064, .T. ) ;
#8311 = DIRECTION ( 'NONE',  ( 0.000000000000000000, 1.000000000000000000, 0.000000000000000000 ) ) ;
#8312 = ITEM_DEFINED_TRANSFORMATION ( 'NONE', 'NONE', #3919,  #594 ) ;
#8313 = EDGE_LOOP ( 'NONE', ( #1475, #7032, #7212, #5638 ) ) ;
#8314 = EDGE_CURVE ( 'NONE', #6891, #5441, #116, .T. ) ;
#8315 = VERTEX_POINT ( 'NONE', #4265 ) ;
#8316 = DIRECTION ( 'NONE',  ( -1.000000000000000000, 0.000000000000000000, -0.000000000000000000 ) ) ;
#8317 = LINE ( 'NONE', #1040, #176 ) ;
#8318 = CARTESIAN_POINT ( 'NONE',  ( -4.000000000000000000, -0.3979232138631226823, -3.896351557369779711E-17 ) ) ;
#8319 = CARTESIAN_POINT ( 'NONE',  ( -0.6666666666666666297, -4.233901974057276973, -3.300726591567087365 ) ) ;
#8320 = ORIENTED_EDGE ( 'NONE', *, *, #7553, .T. ) ;
#8321 = DIRECTION ( 'NONE',  ( -1.214306433183764966E-17, 1.000000000000000000, 0.000000000000000000 ) ) ;
#8322 = DIRECTION ( 'NONE',  ( 0.000000000000000000, 0.000000000000000000, -1.000000000000000000 ) ) ;
#8323 = ORIENTED_EDGE ( 'NONE', *, *, #7519, .T. ) ;
#8324 = VERTEX_POINT ( 'NONE', #207 ) ;
#8325 = LINE ( 'NONE', #2363, #3517 ) ;
#8326 = CIRCLE ( 'NONE', #5525, 0.2000000000000000944 ) ;
#8327 = DIRECTION ( 'NONE',  ( -0.000000000000000000, -0.000000000000000000, 1.000000000000000000 ) ) ;
#8328 = EDGE_CURVE ( 'NONE', #3270, #1117, #1610, .T. ) ;
#8329 = DIRECTION ( 'NONE',  ( -1.000000000000000000, 1.734723475976806848E-16, -0.000000000000000000 ) ) ;
#8330 = FACE_OUTER_BOUND ( 'NONE', #7794, .T. ) ;
#8331 = ORIENTED_EDGE ( 'NONE', *, *, #2299, .T. ) ;
#8332 = PLANE ( 'NONE',  #2641 ) ;
#8333 = EDGE_LOOP ( 'NONE', ( #1966, #4485, #7078, #2780 ) ) ;
#8334 = LINE ( 'NONE', #5748, #5040 ) ;
#8335 = ADVANCED_FACE ( 'NONE', ( #831 ), #881, .T. ) ;
#8336 = VECTOR ( 'NONE', #4967, 1000.000000000000000 ) ;
#8337 = PLANE ( 'NONE',  #4613 ) ;
#8338 = CARTESIAN_POINT ( 'NONE',  ( 0.000000000000000000, 0.000000000000000000, -14.56854249492377207 ) ) ;
#8339 = CARTESIAN_POINT ( 'NONE',  ( -5.000000000000000000, -5.000000000000000000, -97.99999999999997158 ) ) ;
#8340 = CARTESIAN_POINT ( 'NONE',  ( -4.000000000000000000, -2.512220745329312610, -3.469390707569719901 ) ) ;
#8341 = AXIS2_PLACEMENT_3D ( 'NONE', #2357, #996, #5196 ) ;
#8342 = ORIENTED_EDGE ( 'NONE', *, *, #4844, .F. ) ;
#8343 = ORIENTED_EDGE ( 'NONE', *, *, #5629, .T. ) ;
#8344 = EDGE_LOOP ( 'NONE', ( #197, #3276, #6838, #4806 ) ) ;
#8345 = CYLINDRICAL_SURFACE ( 'NONE', #2837, 10.00000000000000000 ) ;
#8346 = DIRECTION ( 'NONE',  ( 1.000000000000000000, 0.000000000000000000, 0.000000000000000000 ) ) ;
#8347 = ORIENTED_EDGE ( 'NONE', *, *, #4994, .F. ) ;
#8348 = LINE ( 'NONE', #4380, #7875 ) ;
#8349 = EDGE_LOOP ( 'NONE', ( #6742, #3303 ) ) ;
#8350 =( NAMED_UNIT ( * ) SI_UNIT ( $, .STERADIAN. ) SOLID_ANGLE_UNIT ( ) );
#8351 = CARTESIAN_POINT ( 'NONE',  ( 5.000000000000000000, 5.000000000000000000, -36.00000000000000000 ) ) ;
#8352 = VECTOR ( 'NONE', #7285, 999.9999999999998863 ) ;
#8353 = CONTEXT_DEPENDENT_SHAPE_REPRESENTATION ( #2143, #2884 ) ;
#8354 = ORIENTED_EDGE ( 'NONE', *, *, #1931, .T. ) ;
#8355 = EDGE_LOOP ( 'NONE', ( #6616, #6732, #4098, #4814 ) ) ;
#8356 = LINE ( 'NONE', #2397, #8015 ) ;
#8357 = CARTESIAN_POINT ( 'NONE',  ( 5.000000000000000000, -5.000000000000000000, -71.99999999999998579 ) ) ;
#8358 = ADVANCED_FACE ( 'NONE', ( #3401 ), #3443, .T. ) ;
#8359 = EDGE_CURVE ( 'NONE', #1490, #3127, #3373, .T. ) ;
#8360 = LINE ( 'NONE', #6997, #2723 ) ;
#8361 = DIRECTION ( 'NONE',  ( 0.000000000000000000, 0.000000000000000000, 1.000000000000000000 ) ) ;
#8362 = ORIENTED_EDGE ( 'NONE', *, *, #5282, .F. ) ;
#8363 = DIRECTION ( 'NONE',  ( 0.000000000000000000, 0.000000000000000000, 1.000000000000000000 ) ) ;
#8364 = DIRECTION ( 'NONE',  ( 1.000000000000000000, 0.000000000000000000, 0.000000000000000000 ) ) ;
#8365 = VERTEX_POINT ( 'NONE', #1332 ) ;
#8366 = ORIENTED_EDGE ( 'NONE', *, *, #11, .T. ) ;
#8367 = DIRECTION ( 'NONE',  ( 1.000000000000000000, -1.734723475976806848E-16, 0.000000000000000000 ) ) ;
#8368 = CARTESIAN_POINT ( 'NONE',  ( 93.00000000000000000, -4.999999999999998224, 139.9990000000000236 ) ) ;
#8369 = EDGE_CURVE ( 'NONE', #5141, #5928, #7135, .T. ) ;
#8370 = DIRECTION ( 'NONE',  ( -0.000000000000000000, 1.000000000000000000, -0.000000000000000000 ) ) ;
#8371 = CARTESIAN_POINT ( 'NONE',  ( 5.000000000000000000, 5.000000000000000000, 7.000000000000006217 ) ) ;
#8372 = ORIENTED_EDGE ( 'NONE', *, *, #5376, .F. ) ;
#8373 =( NAMED_UNIT ( * ) PLANE_ANGLE_UNIT ( ) SI_UNIT ( $, .RADIAN. ) );
#8374 = EDGE_LOOP ( 'NONE', ( #252, #474, #3741, #5468 ) ) ;
#8375 =( REPRESENTATION_RELATIONSHIP ('NONE','NONE', #3312, #1479 ) REPRESENTATION_RELATIONSHIP_WITH_TRANSFORMATION ( #8052 )SHAPE_REPRESENTATION_RELATIONSHIP( ) );
#8376 = CARTESIAN_POINT ( 'NONE',  ( 4.235886605889389145, 2.417314728048528760, -3.751161874094018245 ) ) ;
#8377 =( GEOMETRIC_REPRESENTATION_CONTEXT ( 3 ) GLOBAL_UNCERTAINTY_ASSIGNED_CONTEXT ( ( #8565 ) ) GLOBAL_UNIT_ASSIGNED_CONTEXT ( ( #6551, #7210, #3344 ) ) REPRESENTATION_CONTEXT ( 'NONE', 'WORKASPACE' ) );
#8378 = VECTOR ( 'NONE', #1877, 1000.000000000000000 ) ;
#8379 = FACE_OUTER_BOUND ( 'NONE', #3686, .T. ) ;
#8380 = DIRECTION ( 'NONE',  ( 0.000000000000000000, 0.000000000000000000, -1.000000000000000000 ) ) ;
#8381 = LINE ( 'NONE', #3757, #1395 ) ;
#8382 = CARTESIAN_POINT ( 'NONE',  ( 219.9999999999999716, -15.00000000000000000, 162.5000000000000853 ) ) ;
#8383 = CARTESIAN_POINT ( 'NONE',  ( -5.000000000000000000, -5.000000000000000000, 140.0000000000000000 ) ) ;
#8384 = EDGE_LOOP ( 'NONE', ( #7996, #6240, #6738, #7835 ) ) ;
#8385 = VECTOR ( 'NONE', #2717, 1000.000000000000000 ) ;
#8386 = DIRECTION ( 'NONE',  ( -0.000000000000000000, -0.000000000000000000, 1.000000000000000000 ) ) ;
#8387 = CARTESIAN_POINT ( 'NONE',  ( 303.3333333333333144, -15.00000000000000000, 159.8500000000001080 ) ) ;
#8388 = EDGE_CURVE ( 'NONE', #4780, #8142, #7402, .T. ) ;
#8389 = CARTESIAN_POINT ( 'NONE',  ( 470.0000000000000000, -15.00000000000000000, 180.0000000000000284 ) ) ;
#8390 = UNCERTAINTY_MEASURE_WITH_UNIT (LENGTH_MEASURE( 1.000000000000000082E-05 ), #2957, 'distance_accuracy_value', 'NONE');
#8391 = PRODUCT_DEFINITION_SHAPE ( 'NONE', 'NONE',  #8623 ) ;
#8392 = EDGE_CURVE ( 'NONE', #5734, #1501, #17, .T. ) ;
#8393 = CIRCLE ( 'NONE', #5873, 2.649999999999985700 ) ;
#8394 = EDGE_CURVE ( 'NONE', #4773, #6725, #1991, .T. ) ;
#8395 = ORIENTED_EDGE ( 'NONE', *, *, #7451, .F. ) ;
#8396 = DIRECTION ( 'NONE',  ( 0.000000000000000000, 0.000000000000000000, -1.000000000000000000 ) ) ;
#8397 = VECTOR ( 'NONE', #3555, 1000.000000000000000 ) ;
#8398 = ORIENTED_EDGE ( 'NONE', *, *, #3272, .F. ) ;
#8399 = SURFACE_SIDE_STYLE ('',( #416 ) ) ;
#8400 = VECTOR ( 'NONE', #2996, 1000.000000000000000 ) ;
#8401 = DIRECTION ( 'NONE',  ( 1.000000000000000000, 0.000000000000000000, 0.000000000000000000 ) ) ;
#8402 = ORIENTED_EDGE ( 'NONE', *, *, #6128, .F. ) ;
#8403 = VECTOR ( 'NONE', #1251, 1000.000000000000000 ) ;
#8404 = ORIENTED_EDGE ( 'NONE', *, *, #7008, .F. ) ;
#8405 = FACE_OUTER_BOUND ( 'NONE', #2441, .T. ) ;
#8406 = LINE ( 'NONE', #1080, #8256 ) ;
#8407 = FACE_OUTER_BOUND ( 'NONE', #3090, .T. ) ;
#8408 = EDGE_LOOP ( 'NONE', ( #5324, #6964 ) ) ;
#8409 = EDGE_CURVE ( 'NONE', #3613, #7220, #4685, .T. ) ;
#8410 = CARTESIAN_POINT ( 'NONE',  ( 176.0000000000000000, 0.000000000000000000, 0.000000000000000000 ) ) ;
#8411 = FACE_OUTER_BOUND ( 'NONE', #811, .T. ) ;
#8412 = ORIENTED_EDGE ( 'NONE', *, *, #3296, .F. ) ;
#8413 = ORIENTED_EDGE ( 'NONE', *, *, #5706, .T. ) ;
#8414 = FACE_OUTER_BOUND ( 'NONE', #1879, .T. ) ;
#8415 = CARTESIAN_POINT ( 'NONE',  ( 3.333333333333335702, -2.694301256218268215, -3.300726591567084256 ) ) ;
#8416 = AXIS2_PLACEMENT_3D ( 'NONE', #5345, #1519, #6213 ) ;
#8417 = B_SPLINE_CURVE_WITH_KNOTS ( 'NONE', 3,
 ( #1039, #4426, #6253, #5121, #1650, #4299 ),
 .UNSPECIFIED., .F., .F.,
 ( 4, 2, 4 ),
 ( 0.002452478801916376308, 0.003676905084148007850, 0.004901331366379639391 ),
 .UNSPECIFIED. ) ;
#8418 = FACE_OUTER_BOUND ( 'NONE', #1929, .T. ) ;
#8419 = LINE ( 'NONE', #8371, #6788 ) ;
#8420 = ORIENTED_EDGE ( 'NONE', *, *, #3748, .F. ) ;
#8421 = VERTEX_POINT ( 'NONE', #7343 ) ;
#8422 = DIRECTION ( 'NONE',  ( -0.000000000000000000, -0.000000000000000000, 1.000000000000000000 ) ) ;
#8423 = PRODUCT_RELATED_PRODUCT_CATEGORY ( 'part', '', ( #1270 ) ) ;
#8424 = CARTESIAN_POINT ( 'NONE',  ( 1.734723475976807094E-15, 4.618802153517012954, -0.4999999999999995559 ) ) ;
#8425 = DIRECTION ( 'NONE',  ( -0.000000000000000000, -1.000000000000000000, -0.000000000000000000 ) ) ;
#8426 = DIRECTION ( 'NONE',  ( 0.000000000000000000, 0.000000000000000000, -1.000000000000000000 ) ) ;
#8427 = DIRECTION ( 'NONE',  ( -0.000000000000000000, -0.000000000000000000, 1.000000000000000000 ) ) ;
#8428 = ORIENTED_EDGE ( 'NONE', *, *, #60, .F. ) ;
#8429 = CARTESIAN_POINT ( 'NONE',  ( 10.00000000000000000, 0.000000000000000000, -7.999999999999996447 ) ) ;
#8430 = CARTESIAN_POINT ( 'NONE',  ( -6.473970235329672780E-16, -4.862606272033106691, -3.745885042887442395 ) ) ;
#8431 = CARTESIAN_POINT ( 'NONE',  ( -5.000000000000001776, 5.000000000000001776, -143.0000000000000284 ) ) ;
#8432 = EDGE_CURVE ( 'NONE', #4191, #5694, #7957, .T. ) ;
#8433 = EDGE_LOOP ( 'NONE', ( #1100, #4048, #1370, #3627 ) ) ;
#8434 = CIRCLE ( 'NONE', #8154, 2.041999999999999815 ) ;
#8435 = FILL_AREA_STYLE_COLOUR ( '', #6055 ) ;
#8436 = EDGE_CURVE ( 'NONE', #1609, #6518, #3871, .T. ) ;
#8437 = VECTOR ( 'NONE', #1119, 1000.000000000000000 ) ;
#8438 = ORIENTED_EDGE ( 'NONE', *, *, #7960, .T. ) ;
#8439 = CARTESIAN_POINT ( 'NONE',  ( 5.000000000000000000, -5.000000000000000000, -143.0000000000000284 ) ) ;
#8440 = ADVANCED_FACE ( 'NONE', ( #8528 ), #5164, .T. ) ;
#8441 = CONTEXT_DEPENDENT_SHAPE_REPRESENTATION ( #4633, #233 ) ;
#8442 = ORIENTED_EDGE ( 'NONE', *, *, #7553, .F. ) ;
#8443 = ORIENTED_EDGE ( 'NONE', *, *, #7636, .T. ) ;
#8444 = LINE ( 'NONE', #3604, #8293 ) ;
#8445 = EDGE_CURVE ( 'NONE', #5075, #392, #6138, .T. ) ;
#8446 = CARTESIAN_POINT ( 'NONE',  ( -4.000000000000000000, -2.309401076758515803, -0.4999999999999995559 ) ) ;
#8447 = MECHANICAL_DESIGN_GEOMETRIC_PRESENTATION_REPRESENTATION (  '', ( #3155 ), #7180 ) ;
#8448 = CLOSED_SHELL ( 'NONE', ( #3754, #2845, #3564, #3083, #3042, #167, #753, #1341, #5533, #5865, #6928, #5395, #4459, #7591, #2560, #1699, #986, #7413, #3834, #2758, #7020, #8358, #1152, #5851, #4536, #3720, #2630, #4993, #3766, #1048, #361, #5073, #4730, #6807, #6910, #87, #1129, #2455, #7148, #4591, #984, #1010 ) ) ;
#8449 = CARTESIAN_POINT ( 'NONE',  ( -4.000000000000000000, 0.000000000000000000, 0.000000000000000000 ) ) ;
#8450 = ORIENTED_EDGE ( 'NONE', *, *, #8392, .F. ) ;
#8451 = AXIS2_PLACEMENT_3D ( 'NONE', #114, #7228, #5267 ) ;
#8452 = AXIS2_PLACEMENT_3D ( 'NONE', #4528, #5101, #7727 ) ;
#8453 = CARTESIAN_POINT ( 'NONE',  ( 53.33333333333330017, -10.00000000000000000, 162.5000000000000853 ) ) ;
#8454 = CARTESIAN_POINT ( 'NONE',  ( -5.000000000000000000, -5.000000000000000000, -36.00000000000000000 ) ) ;
#8455 = ORIENTED_EDGE ( 'NONE', *, *, #6366, .T. ) ;
#8456 = ORIENTED_EDGE ( 'NONE', *, *, #3491, .F. ) ;
#8457 = CARTESIAN_POINT ( 'NONE',  ( 5.000000000000000000, 5.000000000000000000, -36.00000000000000000 ) ) ;
#8458 = CARTESIAN_POINT ( 'NONE',  ( 2.500000000000000000, 1.178949249685213863, -2.042000000000001148 ) ) ;
#8459 = FACE_BOUND ( 'NONE', #4556, .T. ) ;
#8460 = DIRECTION ( 'NONE',  ( 0.000000000000000000, 0.000000000000000000, 1.000000000000000000 ) ) ;
#8461 = ORIENTED_EDGE ( 'NONE', *, *, #2493, .T. ) ;
#8462 =( NAMED_UNIT ( * ) SI_UNIT ( $, .STERADIAN. ) SOLID_ANGLE_UNIT ( ) );
#8463 = ORIENTED_EDGE ( 'NONE', *, *, #7490, .T. ) ;
#8464 = LINE ( 'NONE', #1014, #5450 ) ;
#8465 = EDGE_CURVE ( 'NONE', #1114, #2573, #1432, .T. ) ;
#8466 = EDGE_CURVE ( 'NONE', #8098, #5082, #3299, .T. ) ;
#8467 = FACE_BOUND ( 'NONE', #5941, .T. ) ;
#8468 = FACE_OUTER_BOUND ( 'NONE', #5418, .T. ) ;
#8469 = EDGE_CURVE ( 'NONE', #6087, #1828, #3521, .T. ) ;
#8470 = DIRECTION ( 'NONE',  ( 1.000000000000000000, 0.000000000000000000, 0.000000000000000000 ) ) ;
#8471 = FILL_AREA_STYLE ('',( #8109 ) ) ;
#8472 = VECTOR ( 'NONE', #6132, 1000.000000000000000 ) ;
#8473 = DIRECTION ( 'NONE',  ( 0.000000000000000000, 0.000000000000000000, 1.000000000000000000 ) ) ;
#8474 = PLANE ( 'NONE',  #2292 ) ;
#8475 = CARTESIAN_POINT ( 'NONE',  ( 219.9999999999999716, -25.00000000000000000, 162.5000000000000853 ) ) ;
#8476 = EDGE_CURVE ( 'NONE', #6409, #6568, #3214, .T. ) ;
#8477 = CARTESIAN_POINT ( 'NONE',  ( 0.000000000000000000, 0.000000000000000000, 0.000000000000000000 ) ) ;
#8478 = ORIENTED_EDGE ( 'NONE', *, *, #2533, .F. ) ;
#8479 = DIRECTION ( 'NONE',  ( 0.000000000000000000, 0.000000000000000000, 1.000000000000000000 ) ) ;
#8480 = VERTEX_POINT ( 'NONE', #4609 ) ;
#8481 = CARTESIAN_POINT ( 'NONE',  ( 5.000000000000000000, 5.000000000000000000, -71.99999999999998579 ) ) ;
#8482 = CIRCLE ( 'NONE', #6093, 5.384454397937118664 ) ;
#8483 = LINE ( 'NONE', #5642, #3800 ) ;
#8484 = DIRECTION ( 'NONE',  ( 0.000000000000000000, 0.000000000000000000, 1.000000000000000000 ) ) ;
#8485 = AXIS2_PLACEMENT_3D ( 'NONE', #3016, #671, #6755 ) ;
#8486 = VERTEX_POINT ( 'NONE', #1914 ) ;
#8487 = CARTESIAN_POINT ( 'NONE',  ( 4.203833317240879275, 1.627343821129582979, -3.597273115243889929 ) ) ;
#8488 = ADVANCED_FACE ( 'NONE', ( #4551 ), #6639, .F. ) ;
#8489 = DIRECTION ( 'NONE',  ( 1.000000000000000000, 0.000000000000000000, 0.000000000000000000 ) ) ;
#8490 = FACE_OUTER_BOUND ( 'NONE', #7505, .T. ) ;
#8491 = VERTEX_POINT ( 'NONE', #5287 ) ;
#8492 = VERTEX_POINT ( 'NONE', #4639 ) ;
#8493 = DIRECTION ( 'NONE',  ( 1.000000000000000000, 0.000000000000000000, 0.000000000000000000 ) ) ;
#8494 = CARTESIAN_POINT ( 'NONE',  ( 93.00000000000000000, -4.999999999999998224, 145.0000000000000284 ) ) ;
#8495 = FACE_OUTER_BOUND ( 'NONE', #6251, .T. ) ;
#8496 = CARTESIAN_POINT ( 'NONE',  ( 0.000000000000000000, 0.000000000000000000, -36.00000000000000000 ) ) ;
#8497 = VERTEX_POINT ( 'NONE', #7250 ) ;
#8498 = EDGE_CURVE ( 'NONE', #6221, #8107, #1249, .T. ) ;
#8499 =( NAMED_UNIT ( * ) PLANE_ANGLE_UNIT ( ) SI_UNIT ( $, .RADIAN. ) );
#8500 = VERTEX_POINT ( 'NONE', #5246 ) ;
#8501 = PLANE ( 'NONE',  #7541 ) ;
#8502 = CARTESIAN_POINT ( 'NONE',  ( 2.649999999999993694, 157.5000000000000284, 0.000000000000000000 ) ) ;
#8503 = DIRECTION ( 'NONE',  ( 1.000000000000000000, 0.000000000000000000, 0.000000000000000000 ) ) ;
#8504 = LINE ( 'NONE', #7810, #3608 ) ;
#8505 = PLANE ( 'NONE',  #7336 ) ;
#8506 = EDGE_CURVE ( 'NONE', #437, #8491, #34, .T. ) ;
#8507 = CARTESIAN_POINT ( 'NONE',  ( -4.999999999999998224, 5.000000000000001776, 139.9990000000000236 ) ) ;
#8508 = CARTESIAN_POINT ( 'NONE',  ( 0.000000000000000000, 0.000000000000000000, 120.0000000000000142 ) ) ;
#8509 = CARTESIAN_POINT ( 'NONE',  ( 4.024499207728657879, -2.323545700935587988, -3.572172305156509964 ) ) ;
#8510 = AXIS2_PLACEMENT_3D ( 'NONE', #20, #1999, #728 ) ;
#8511 = CIRCLE ( 'NONE', #865, 20.00000000000000000 ) ;
#8512 = CARTESIAN_POINT ( 'NONE',  ( 4.024499207728657879, 2.323545700935571556, -3.572172305156506411 ) ) ;
#8513 = CARTESIAN_POINT ( 'NONE',  ( 20.00000000000000000, 0.000000000000000000, 62.00000000000001421 ) ) ;
#8514 = ORIENTED_EDGE ( 'NONE', *, *, #1994, .F. ) ;
#8515 =( NAMED_UNIT ( * ) SI_UNIT ( $, .STERADIAN. ) SOLID_ANGLE_UNIT ( ) );
#8516 = DIRECTION ( 'NONE',  ( 1.000000000000000000, 0.000000000000000000, -0.000000000000000000 ) ) ;
#8517 = VERTEX_POINT ( 'NONE', #641 ) ;
#8518 = CARTESIAN_POINT ( 'NONE',  ( 5.000000000000000000, -5.000000000000000000, -71.99999999999998579 ) ) ;
#8519 = CIRCLE ( 'NONE', #7401, 10.00000000000000000 ) ;
#8520 = CARTESIAN_POINT ( 'NONE',  ( 386.6666666666666288, -15.00000000000000000, 159.8500000000001080 ) ) ;
#8521 = EDGE_CURVE ( 'NONE', #4515, #6932, #6204, .T. ) ;
#8522 = AXIS2_PLACEMENT_3D ( 'NONE', #5463, #6160, #5508 ) ;
#8523 = VECTOR ( 'NONE', #6818, 1000.000000000000000 ) ;
#8524 = CARTESIAN_POINT ( 'NONE',  ( 0.000000000000000000, 0.000000000000000000, -5.000000000000000000 ) ) ;
#8525 = PRODUCT_DEFINITION_SHAPE ( 'NONE', 'NONE',  #8631 ) ;
#8526 = ORIENTED_EDGE ( 'NONE', *, *, #60, .T. ) ;
#8527 = CIRCLE ( 'NONE', #1989, 2.649999999999985700 ) ;
#8528 = FACE_OUTER_BOUND ( 'NONE', #8243, .T. ) ;
#8529 = DIRECTION ( 'NONE',  ( 0.9927523994029856524, -3.078344721374534051E-17, 0.1201776746305850407 ) ) ;
#8530 = LINE ( 'NONE', #1916, #3109 ) ;
#8531 = ORIENTED_EDGE ( 'NONE', *, *, #4704, .T. ) ;
#8532 = VECTOR ( 'NONE', #6896, 1000.000000000000000 ) ;
#8533 = VERTEX_POINT ( 'NONE', #193 ) ;
#8534 = STYLED_ITEM ( 'NONE', ( #2561 ), #1176 ) ;
#8535 = PLANE ( 'NONE',  #1871 ) ;
#8536 = DIRECTION ( 'NONE',  ( -0.000000000000000000, -0.000000000000000000, 1.000000000000000000 ) ) ;
#8537 =( REPRESENTATION_RELATIONSHIP ('NONE','NONE', #3312, #4754 ) REPRESENTATION_RELATIONSHIP_WITH_TRANSFORMATION ( #6466 )SHAPE_REPRESENTATION_RELATIONSHIP( ) );
#8538 = AXIS2_PLACEMENT_3D ( 'NONE', #6895, #6978, #1028 ) ;
#8539 = CYLINDRICAL_SURFACE ( 'NONE', #6330, 2.649999999999985700 ) ;
#8540 = CARTESIAN_POINT ( 'NONE',  ( -4.999999999999998224, 140.0000000000000000, 25.00000000000000000 ) ) ;
#8541 = VERTEX_POINT ( 'NONE', #2815 ) ;
#8542 = ADVANCED_FACE ( 'NONE', ( #7383 ), #8138, .T. ) ;
#8543 = EDGE_CURVE ( 'NONE', #1009, #3640, #5869, .T. ) ;
#8544 = SURFACE_STYLE_USAGE ( .BOTH. , #3229 ) ;
#8545 = ORIENTED_EDGE ( 'NONE', *, *, #4923, .T. ) ;
#8546 = CARTESIAN_POINT ( 'NONE',  ( -5.000000000000001776, 5.000000000000001776, 148.0000000000000284 ) ) ;
#8547 = EDGE_CURVE ( 'NONE', #530, #3444, #1159, .T. ) ;
#8548 = AXIS2_PLACEMENT_3D ( 'NONE', #3095, #3264, #5904 ) ;
#8549 = EDGE_CURVE ( 'NONE', #832, #2080, #6068, .T. ) ;
#8550 = CARTESIAN_POINT ( 'NONE',  ( 2.500000000000000000, -1.178949249685213863, 2.042000000000002924 ) ) ;
#8551 = DIRECTION ( 'NONE',  ( -1.000000000000000000, 0.000000000000000000, 0.000000000000000000 ) ) ;
#8552 = CARTESIAN_POINT ( 'NONE',  ( 5.000000000000000000, -5.000000000000000000, 148.0000000000000284 ) ) ;
#8553 = CARTESIAN_POINT ( 'NONE',  ( 303.3333333333333144, -20.00000000000000000, 162.5000000000000853 ) ) ;
#8554 = DIRECTION ( 'NONE',  ( 0.000000000000000000, 0.000000000000000000, 1.000000000000000000 ) ) ;
#8555 = EDGE_CURVE ( 'NONE', #596, #7097, #5113, .T. ) ;
#8556 = DIRECTION ( 'NONE',  ( 0.000000000000000000, 0.000000000000000000, -1.000000000000000000 ) ) ;
#8557 = FILL_AREA_STYLE ('',( #4 ) ) ;
#8558 = ORIENTED_EDGE ( 'NONE', *, *, #5331, .T. ) ;
#8559 = APPLICATION_PROTOCOL_DEFINITION ( 'draft international standard', 'automotive_design', 1998, #7028 ) ;
#8560 = DIRECTION ( 'NONE',  ( -0.000000000000000000, 1.000000000000000000, -0.000000000000000000 ) ) ;
#8561 = CONTEXT_DEPENDENT_SHAPE_REPRESENTATION ( #4800, #8525 ) ;
#8562 = ORIENTED_EDGE ( 'NONE', *, *, #8394, .T. ) ;
#8563 = LINE ( 'NONE', #3951, #7656 ) ;
#8564 = CARTESIAN_POINT ( 'NONE',  ( 1.312671235360372224, 3.860931062424219462, -0.05923475698270440348 ) ) ;
#8565 = UNCERTAINTY_MEASURE_WITH_UNIT (LENGTH_MEASURE( 1.000000000000000082E-05 ), #6551, 'distance_accuracy_value', 'NONE');
#8566 = AXIS2_PLACEMENT_3D ( 'NONE', #4956, #867, #8103 ) ;
#8567 = EDGE_CURVE ( 'NONE', #7348, #732, #4817, .T. ) ;
#8568 = ADVANCED_FACE ( 'NONE', ( #2775 ), #2962, .T. ) ;
#8569 = DIRECTION ( 'NONE',  ( 0.000000000000000000, 0.000000000000000000, 1.000000000000000000 ) ) ;
#8570 = VERTEX_POINT ( 'NONE', #4038 ) ;
#8571 = CARTESIAN_POINT ( 'NONE',  ( -30.00000000000000000, -15.00000000000000000, 145.0000000000000284 ) ) ;
#8572 = EDGE_CURVE ( 'NONE', #3592, #863, #62, .T. ) ;
#8573 = DIRECTION ( 'NONE',  ( 2.688821387764050996E-17, -1.000000000000000000, -5.551115123125782702E-17 ) ) ;
#8574 = FACE_BOUND ( 'NONE', #5897, .T. ) ;
#8575 = EDGE_LOOP ( 'NONE', ( #4876, #1217, #6489, #7301 ) ) ;
#8576 = ORIENTED_EDGE ( 'NONE', *, *, #5409, .T. ) ;
#8577 = CIRCLE ( 'NONE', #5358, 2.055000000000000160 ) ;
#8578 = DIRECTION ( 'NONE',  ( -1.000000000000000000, -0.000000000000000000, -0.000000000000000000 ) ) ;
#8579 = FACE_BOUND ( 'NONE', #6329, .T. ) ;
#8580 = MECHANICAL_DESIGN_GEOMETRIC_PRESENTATION_REPRESENTATION (  '', ( #3293 ), #6484 ) ;
#8581 = FACE_OUTER_BOUND ( 'NONE', #1031, .T. ) ;
#8582 = AXIS2_PLACEMENT_3D ( 'NONE', #4462, #3124, #543 ) ;
#8583 = PRODUCT ( 'side rail', 'side rail', '', ( #4252 ) ) ;
#8584 = CARTESIAN_POINT ( 'NONE',  ( 176.0000000000000000, -20.00000000000000000, -86.63142504031547730 ) ) ;
#8585 = EDGE_LOOP ( 'NONE', ( #2689, #8213, #2163, #7782 ) ) ;
#8586 = SURFACE_STYLE_FILL_AREA ( #5870 ) ;
#8587 = VERTEX_POINT ( 'NONE', #8094 ) ;
#8588 = FACE_OUTER_BOUND ( 'NONE', #8193, .T. ) ;
#8589 = EDGE_CURVE ( 'NONE', #1611, #1823, #4859, .T. ) ;
#8590 = PLANE ( 'NONE',  #6058 ) ;
#8591 = DIRECTION ( 'NONE',  ( -0.000000000000000000, -0.000000000000000000, 1.000000000000000000 ) ) ;
#8592 = VERTEX_POINT ( 'NONE', #8050 ) ;
#8593 = CARTESIAN_POINT ( 'NONE',  ( -4.101948962585906244, 2.368261337751074169, -3.681124513963621503 ) ) ;
#8594 = CARTESIAN_POINT ( 'NONE',  ( 136.6666666666666288, -20.00000000000000000, 165.1500000000000625 ) ) ;
#8595 = EDGE_CURVE ( 'NONE', #5082, #3699, #6678, .T. ) ;
#8596 = DIRECTION ( 'NONE',  ( -1.000000000000000000, 0.000000000000000000, -0.000000000000000000 ) ) ;
#8597 = CARTESIAN_POINT ( 'NONE',  ( -4.999999999999998224, -4.999999999999998224, 140.0000000000000000 ) ) ;
#8598 = FACE_OUTER_BOUND ( 'NONE', #1819, .T. ) ;
#8599 = PLANE ( 'NONE',  #5142 ) ;
#8600 = DIRECTION ( 'NONE',  ( -1.000000000000000000, 0.000000000000000000, 0.000000000000000000 ) ) ;
#8601 = NEXT_ASSEMBLY_USAGE_OCCURRENCE ( 'NAUO1', ' ', ' ', #5006, #424, $ ) ;
#8602 = NEXT_ASSEMBLY_USAGE_OCCURRENCE ( 'NAUO2', ' ', ' ', #5006, #2614, $ ) ;
#8603 = NEXT_ASSEMBLY_USAGE_OCCURRENCE ( 'NAUO3', ' ', ' ', #5006, #3515, $ ) ;
#8604 = NEXT_ASSEMBLY_USAGE_OCCURRENCE ( 'NAUO4', ' ', ' ', #5006, #6591, $ ) ;
#8605 = NEXT_ASSEMBLY_USAGE_OCCURRENCE ( 'NAUO5', ' ', ' ', #5006, #6591, $ ) ;
#8606 = NEXT_ASSEMBLY_USAGE_OCCURRENCE ( 'NAUO6', ' ', ' ', #5006, #6591, $ ) ;
#8607 = NEXT_ASSEMBLY_USAGE_OCCURRENCE ( 'NAUO7', ' ', ' ', #5006, #6591, $ ) ;
#8608 = NEXT_ASSEMBLY_USAGE_OCCURRENCE ( 'NAUO8', ' ', ' ', #5006, #6591, $ ) ;
#8609 = NEXT_ASSEMBLY_USAGE_OCCURRENCE ( 'NAUO9', ' ', ' ', #5006, #7879, $ ) ;
#8610 = NEXT_ASSEMBLY_USAGE_OCCURRENCE ( 'NAUO10', ' ', ' ', #5006, #7879, $ ) ;
#8611 = NEXT_ASSEMBLY_USAGE_OCCURRENCE ( 'NAUO11', ' ', ' ', #5006, #7879, $ ) ;
#8612 = NEXT_ASSEMBLY_USAGE_OCCURRENCE ( 'NAUO12', ' ', ' ', #5006, #7879, $ ) ;
#8613 = NEXT_ASSEMBLY_USAGE_OCCURRENCE ( 'NAUO13', ' ', ' ', #5006, #7879, $ ) ;
#8614 = NEXT_ASSEMBLY_USAGE_OCCURRENCE ( 'NAUO14', ' ', ' ', #5006, #4792, $ ) ;
#8615 = NEXT_ASSEMBLY_USAGE_OCCURRENCE ( 'NAUO15', ' ', ' ', #5006, #4792, $ ) ;
#8616 = NEXT_ASSEMBLY_USAGE_OCCURRENCE ( 'NAUO16', ' ', ' ', #5006, #4792, $ ) ;
#8617 = NEXT_ASSEMBLY_USAGE_OCCURRENCE ( 'NAUO17', ' ', ' ', #5006, #4792, $ ) ;
#8618 = NEXT_ASSEMBLY_USAGE_OCCURRENCE ( 'NAUO18', ' ', ' ', #5006, #4792, $ ) ;
#8619 = NEXT_ASSEMBLY_USAGE_OCCURRENCE ( 'NAUO19', ' ', ' ', #5006, #4792, $ ) ;
#8620 = NEXT_ASSEMBLY_USAGE_OCCURRENCE ( 'NAUO20', ' ', ' ', #5006, #7502, $ ) ;
#8621 = NEXT_ASSEMBLY_USAGE_OCCURRENCE ( 'NAUO21', ' ', ' ', #5006, #3780, $ ) ;
#8622 = NEXT_ASSEMBLY_USAGE_OCCURRENCE ( 'NAUO22', ' ', ' ', #5006, #7229, $ ) ;
#8623 = NEXT_ASSEMBLY_USAGE_OCCURRENCE ( 'NAUO23', ' ', ' ', #5006, #2571, $ ) ;
#8624 = NEXT_ASSEMBLY_USAGE_OCCURRENCE ( 'NAUO24', ' ', ' ', #5006, #1825, $ ) ;
#8625 = NEXT_ASSEMBLY_USAGE_OCCURRENCE ( 'NAUO25', ' ', ' ', #5006, #6591, $ ) ;
#8626 = NEXT_ASSEMBLY_USAGE_OCCURRENCE ( 'NAUO26', ' ', ' ', #5006, #6591, $ ) ;
#8627 = NEXT_ASSEMBLY_USAGE_OCCURRENCE ( 'NAUO27', ' ', ' ', #5006, #6591, $ ) ;
#8628 = NEXT_ASSEMBLY_USAGE_OCCURRENCE ( 'NAUO28', ' ', ' ', #5006, #6591, $ ) ;
#8629 = NEXT_ASSEMBLY_USAGE_OCCURRENCE ( 'NAUO29', ' ', ' ', #5006, #6591, $ ) ;
#8630 = NEXT_ASSEMBLY_USAGE_OCCURRENCE ( 'NAUO30', ' ', ' ', #5006, #6591, $ ) ;
#8631 = NEXT_ASSEMBLY_USAGE_OCCURRENCE ( 'NAUO31', ' ', ' ', #5006, #7879, $ ) ;
#8632 = NEXT_ASSEMBLY_USAGE_OCCURRENCE ( 'NAUO32', ' ', ' ', #5006, #7879, $ ) ;
#8633 = NEXT_ASSEMBLY_USAGE_OCCURRENCE ( 'NAUO33', ' ', ' ', #5006, #7879, $ ) ;
#8634 = NEXT_ASSEMBLY_USAGE_OCCURRENCE ( 'NAUO34', ' ', ' ', #5006, #7879, $ ) ;
#8635 = NEXT_ASSEMBLY_USAGE_OCCURRENCE ( 'NAUO35', ' ', ' ', #5006, #7879, $ ) ;
#8636 = NEXT_ASSEMBLY_USAGE_OCCURRENCE ( 'NAUO36', ' ', ' ', #5006, #7879, $ ) ;
#8637=COLOUR_RGB('Dark Blue',0.08,0.2,0.34);
#8638=FILL_AREA_STYLE_COLOUR('',#8637);
#8639=FILL_AREA_STYLE('',(#8638));
#8640=SURFACE_STYLE_FILL_AREA(#8639);
#8641=SURFACE_SIDE_STYLE('',(#8640));
#8642=SURFACE_STYLE_USAGE(.BOTH.,#8641);
#8643=PRESENTATION_STYLE_ASSIGNMENT((#8642));
#8644=COLOUR_RGB('Light Blue',0.38,0.62,0.78);
#8645=FILL_AREA_STYLE_COLOUR('',#8644);
#8646=FILL_AREA_STYLE('',(#8645));
#8647=SURFACE_STYLE_FILL_AREA(#8646);
#8648=SURFACE_SIDE_STYLE('',(#8647));
#8649=SURFACE_STYLE_USAGE(.BOTH.,#8648);
#8650=PRESENTATION_STYLE_ASSIGNMENT((#8649));
#8651=COLOUR_RGB('Sky Blue',0.24,0.69,0.87);
#8652=FILL_AREA_STYLE_COLOUR('',#8651);
#8653=FILL_AREA_STYLE('',(#8652));
#8654=SURFACE_STYLE_FILL_AREA(#8653);
#8655=SURFACE_SIDE_STYLE('',(#8654));
#8656=SURFACE_STYLE_USAGE(.BOTH.,#8655);
#8657=PRESENTATION_STYLE_ASSIGNMENT((#8656));
#8658=COLOUR_RGB('Grey',0.48,0.52,0.57);
#8659=FILL_AREA_STYLE_COLOUR('',#8658);
#8660=FILL_AREA_STYLE('',(#8659));
#8661=SURFACE_STYLE_FILL_AREA(#8660);
#8662=SURFACE_SIDE_STYLE('',(#8661));
#8663=SURFACE_STYLE_USAGE(.BOTH.,#8662);
#8664=PRESENTATION_STYLE_ASSIGNMENT((#8663));
#8665=COLOUR_RGB('Black',0.12,0.14,0.17);
#8666=FILL_AREA_STYLE_COLOUR('',#8665);
#8667=FILL_AREA_STYLE('',(#8666));
#8668=SURFACE_STYLE_FILL_AREA(#8667);
#8669=SURFACE_SIDE_STYLE('',(#8668));
#8670=SURFACE_STYLE_USAGE(.BOTH.,#8669);
#8671=PRESENTATION_STYLE_ASSIGNMENT((#8670));
#8672=COLOUR_RGB('Off White',0.89,0.88,0.83);
#8673=FILL_AREA_STYLE_COLOUR('',#8672);
#8674=FILL_AREA_STYLE('',(#8673));
#8675=SURFACE_STYLE_FILL_AREA(#8674);
#8676=SURFACE_SIDE_STYLE('',(#8675));
#8677=SURFACE_STYLE_USAGE(.BOTH.,#8676);
#8678=PRESENTATION_STYLE_ASSIGNMENT((#8677));
ENDSEC;
END-ISO-10303-21;
